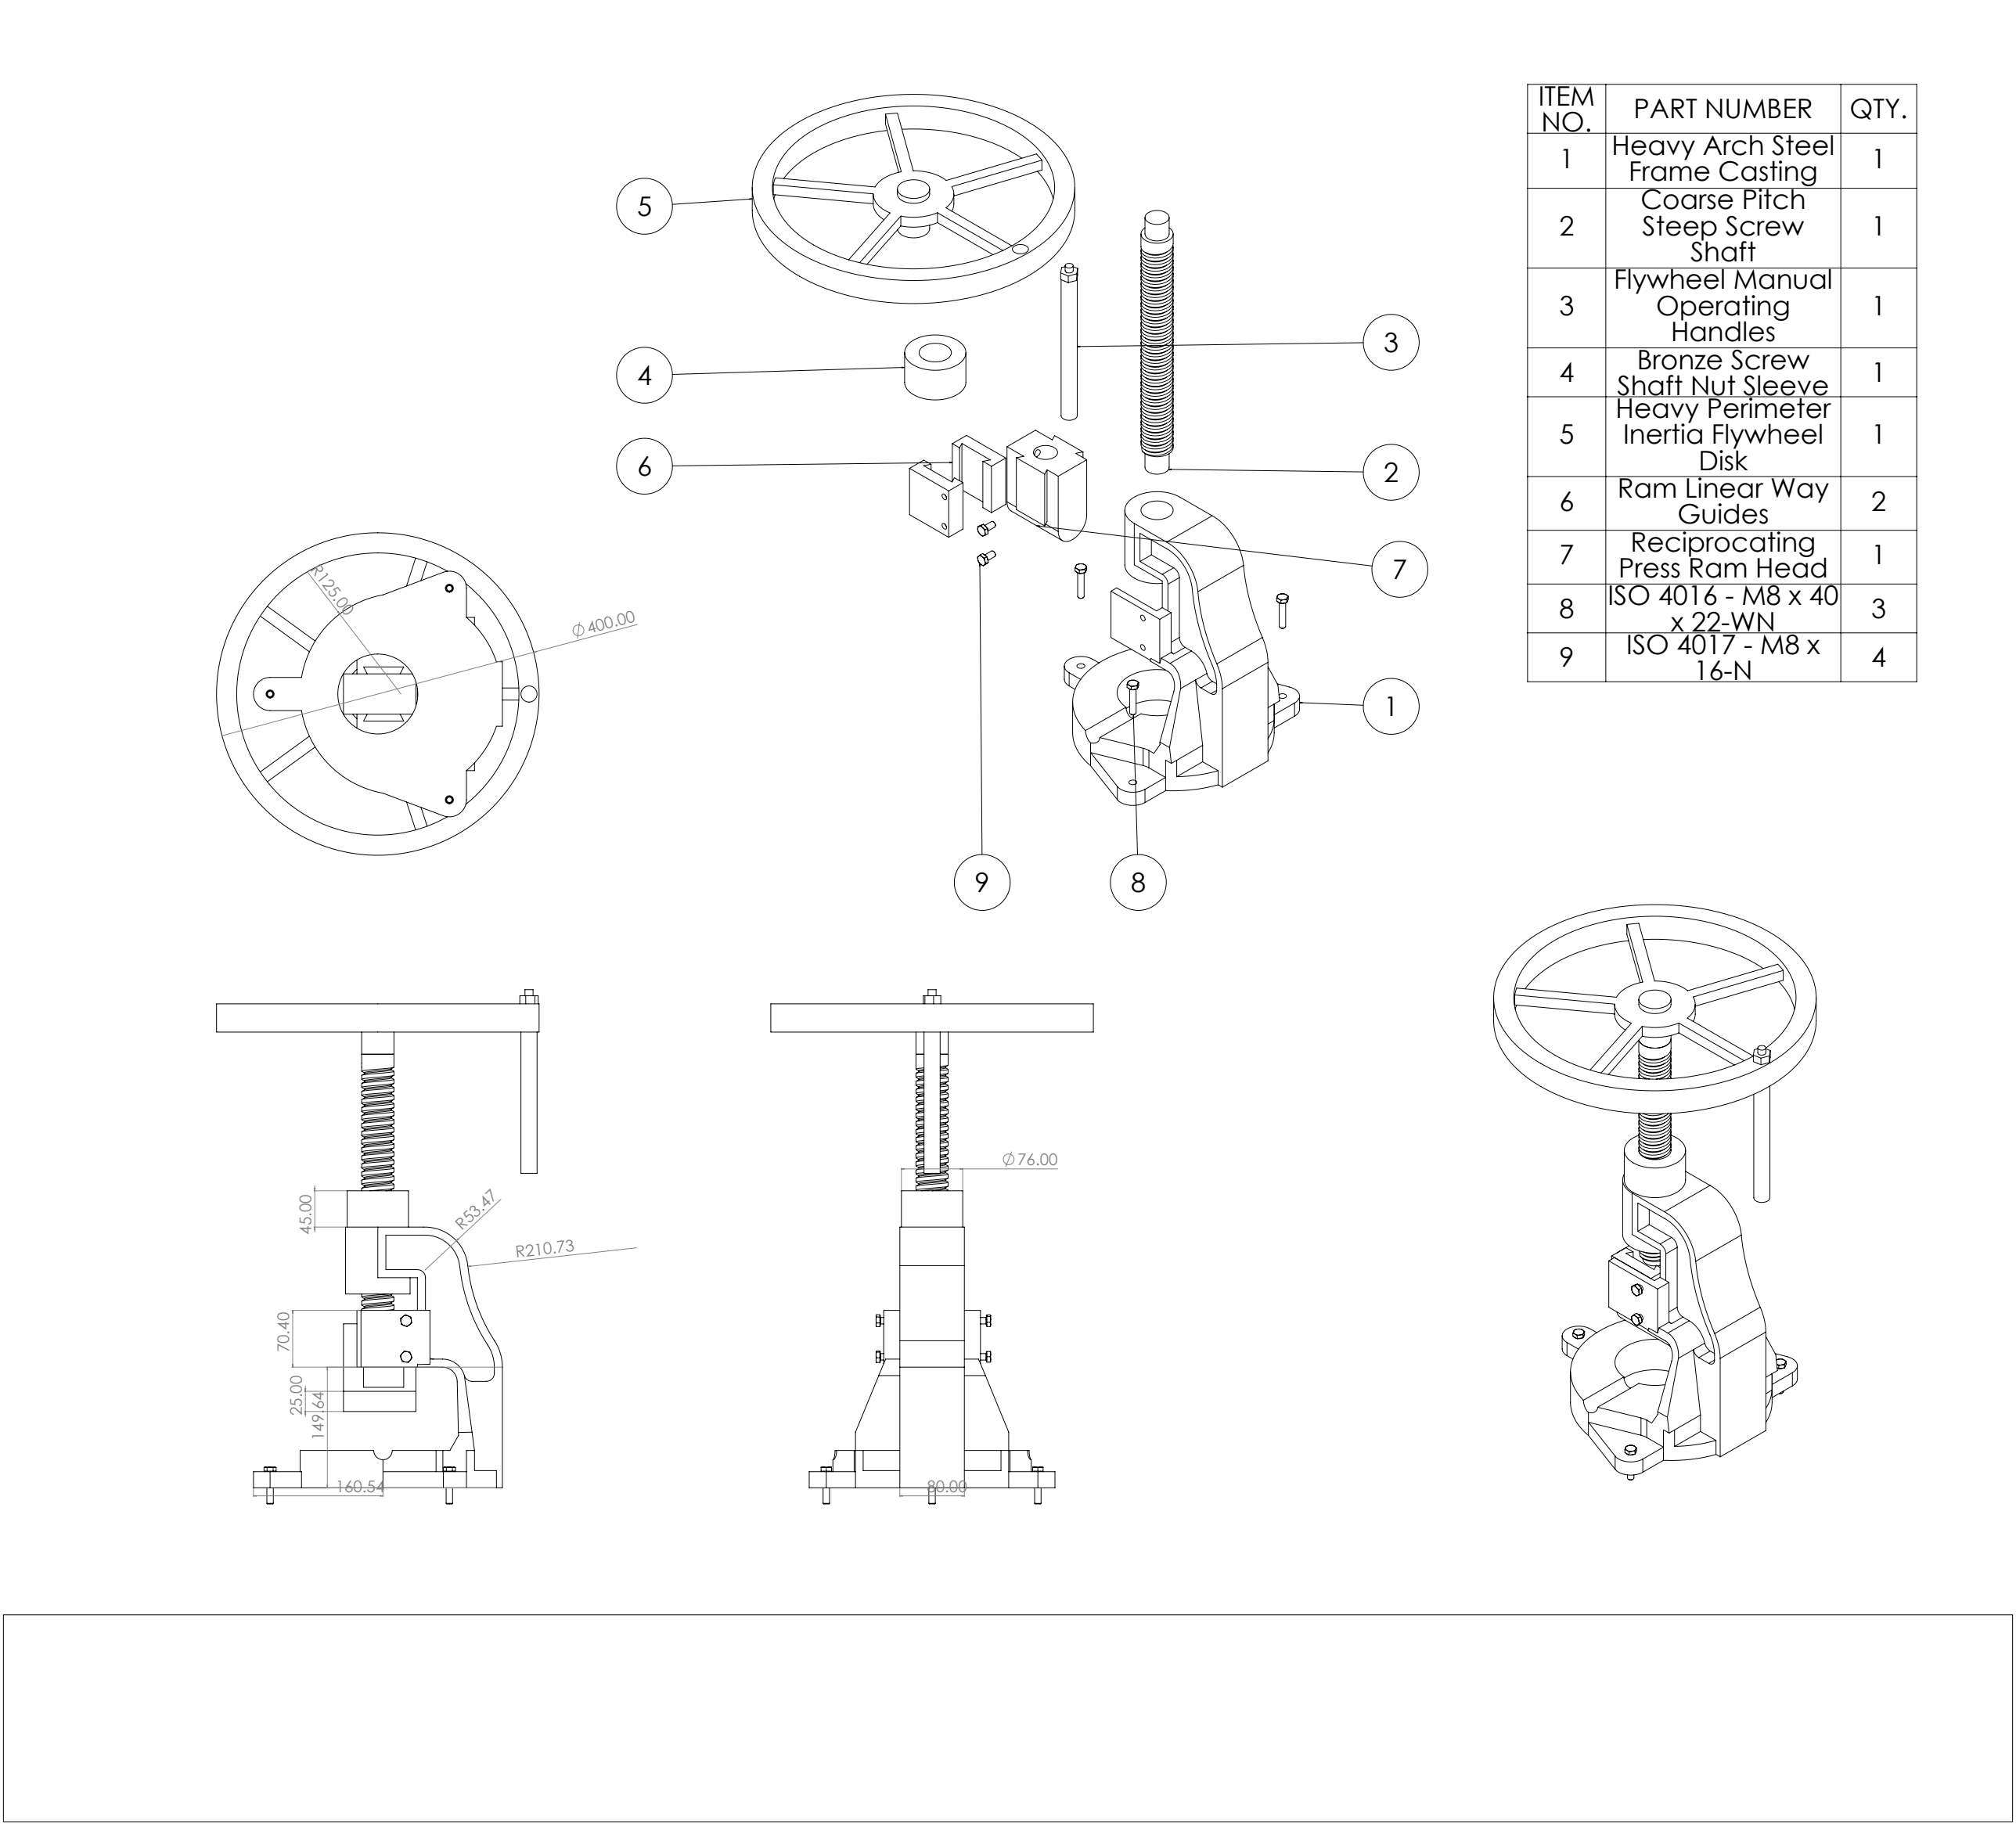
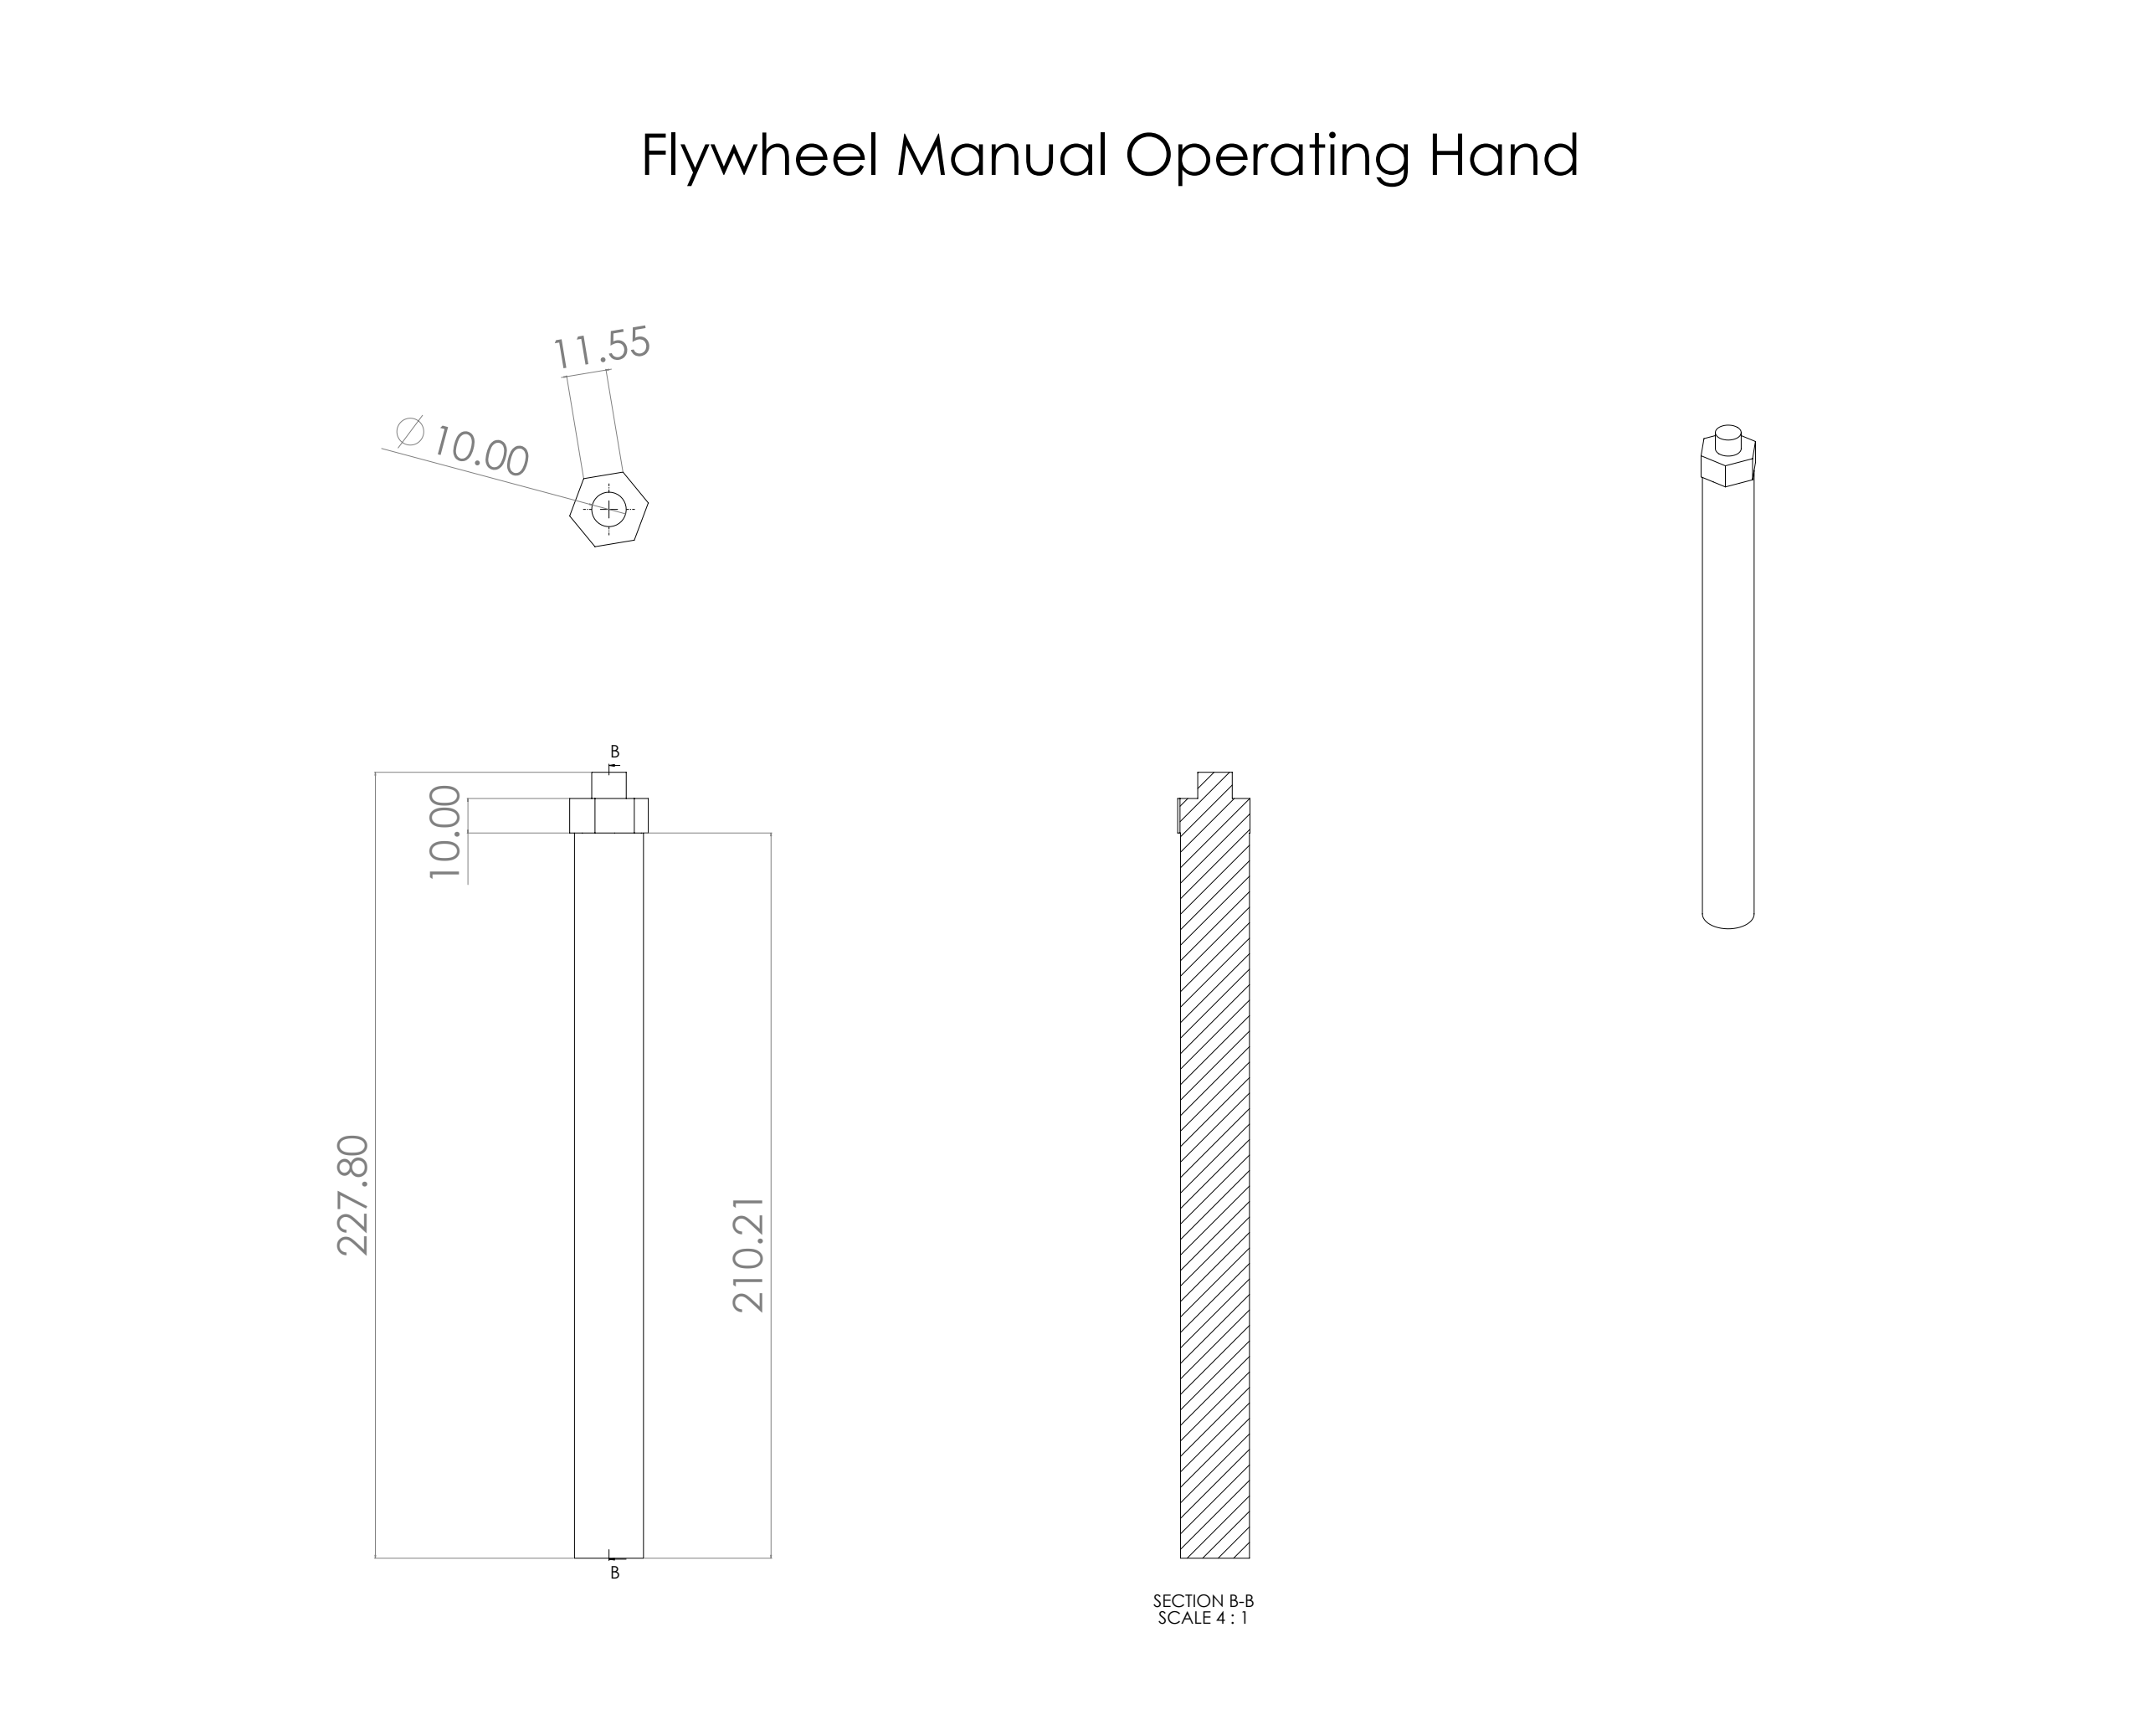
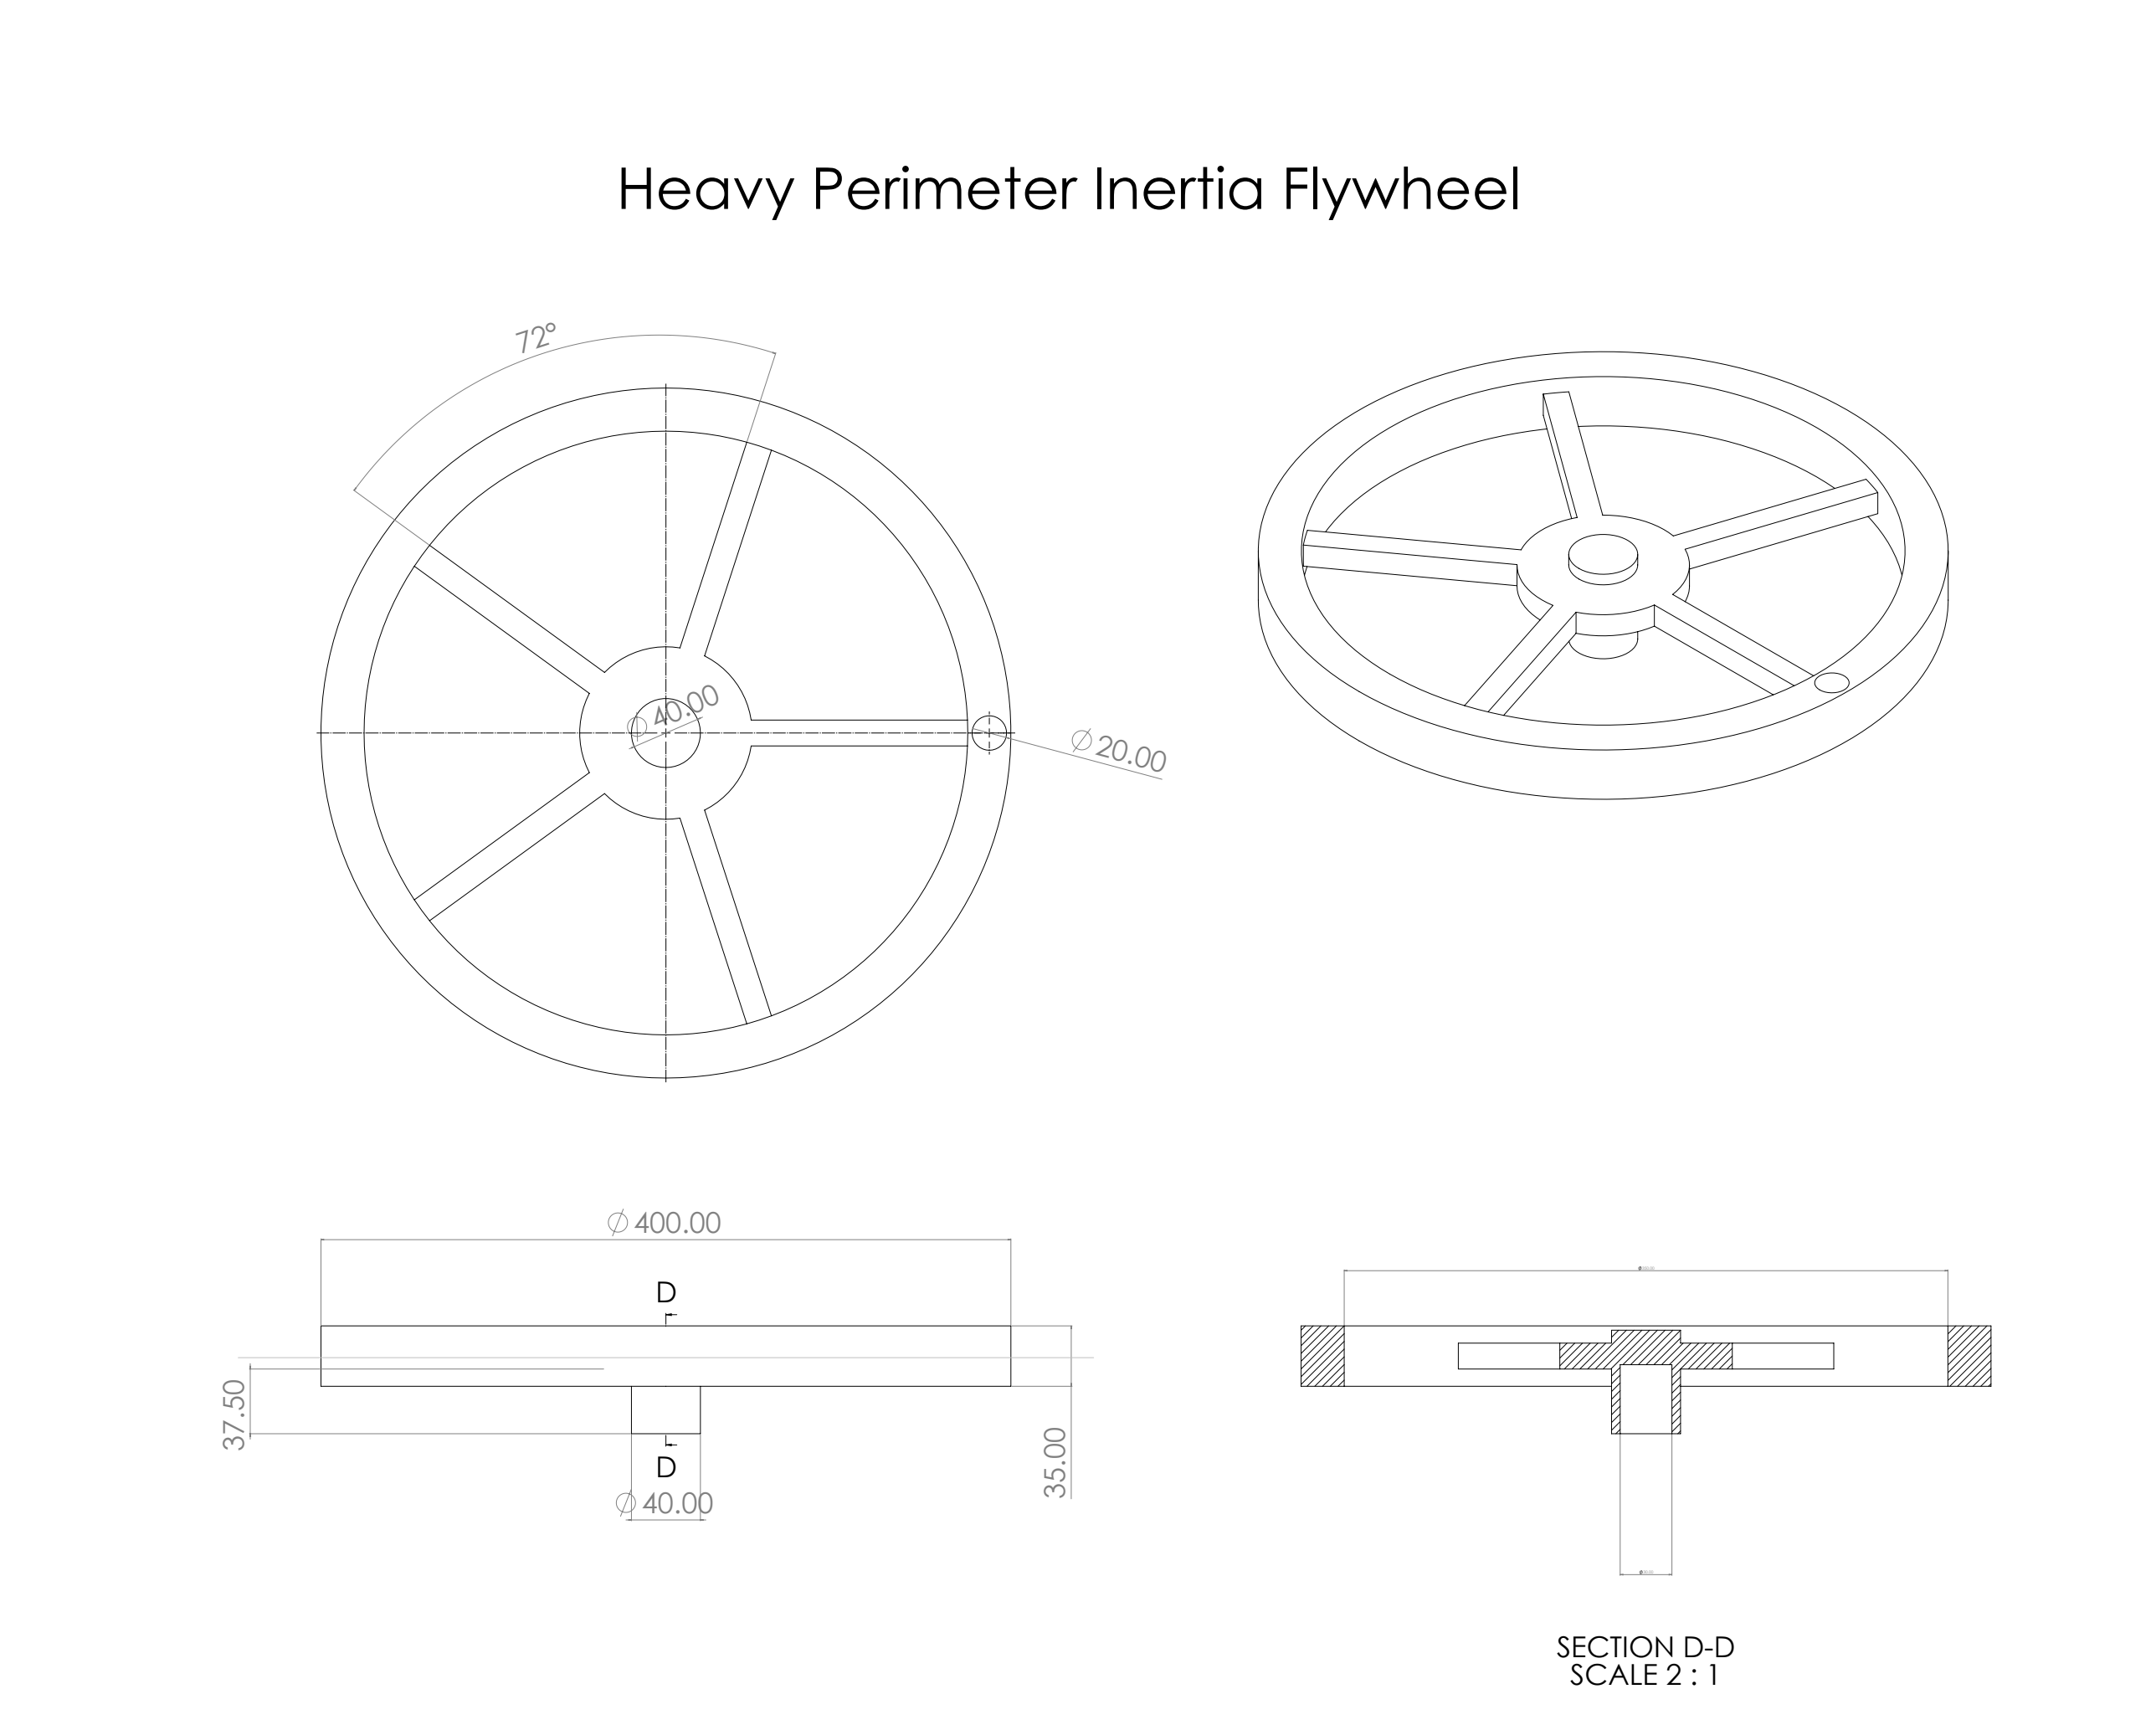
ISO-10303-21;
HEADER;
FILE_DESCRIPTION (('STEP AP214'),
    '1' );
FILE_NAME ('MAS-323',
    '2026-10-24T00:28:05',
    ( '' ),
    ( '' ),
    'SwSTEP 2.0',
    'SolidWorks 2025',
    '' );
FILE_SCHEMA (( 'AUTOMOTIVE_DESIGN' ));
ENDSEC;

DATA;
#1 = CARTESIAN_POINT ( 'NONE',  ( -40.53162694259543031, 272.6198905683720568, -11.84573899990672707 ) ) ;
#2 = CARTESIAN_POINT ( 'NONE',  ( -13.20868407381886200, 380.9948905683720568, -6.410867750099233042 ) ) ;
#3 = VECTOR ( 'NONE', #11444, 1000.000000000000000 ) ;
#4 = DIRECTION ( 'NONE',  ( 0.000000000000000000, -1.000000000000000000, 0.000000000000000000 ) ) ;
#5 = FACE_BOUND ( 'NONE', #9195, .T. ) ;
#6 = CARTESIAN_POINT ( 'NONE',  ( -10.20829729246297646, 267.6198905765655809, -7.653668647301794969 ) ) ;
#7 = CARTESIAN_POINT ( 'NONE',  ( -42.88789093042844058, 432.9323905683720000, -9.489475012073736337 ) ) ;
#8 = DIRECTION ( 'NONE',  ( -0.000000000000000000, -0.000000000000000000, -1.000000000000000000 ) ) ;
#9 = ORIENTED_EDGE ( 'NONE', *, *, #63, .F. ) ;
#10 = CARTESIAN_POINT ( 'NONE',  ( -47.16347859291445133, 436.6198905601784759, -7.653668647301793193 ) ) ;
#11 = ORIENTED_EDGE ( 'NONE', *, *, #16208, .F. ) ;
#12 = ORIENTED_EDGE ( 'NONE', *, *, #11019, .T. ) ;
#13 = VERTEX_POINT ( 'NONE', #14894 ) ;
#14 = CARTESIAN_POINT ( 'NONE',  ( -43.04716123355245827, 207.6569251493015429, -4.334626618252813479 ) ) ;
#15 = CARTESIAN_POINT ( 'NONE',  ( -40.01497788969912506, 298.8073905601784759, 16.95518130045146776 ) ) ;
#16 = FACE_OUTER_BOUND ( 'NONE', #20943, .T. ) ;
#17 = CARTESIAN_POINT ( 'NONE',  ( -40.53162694259543741, 334.1198905683720568, -11.84573899990672707 ) ) ;
#18 = CARTESIAN_POINT ( 'NONE',  ( -48.68588794268872277, 492.3073905765656946, 3.978247347593168115 ) ) ;
#19 = CARTESIAN_POINT ( 'NONE',  ( -25.35362745456398059, 366.6823905683720000, 16.75240474999998952 ) ) ;
#20 = CARTESIAN_POINT ( 'NONE',  ( -28.68588794268870856, 309.4948905765656377, -19.99999999999999289 ) ) ;
#21 = CARTESIAN_POINT ( 'NONE',  ( -11.93348319268872437, 388.5573905683719431, 3.332260488124728859 ) ) ;
#22 = CARTESIAN_POINT ( 'NONE',  ( -36.33955658999050087, 300.1198905765656377, -18.47759065022572855 ) ) ;
#23 = CARTESIAN_POINT ( 'NONE',  ( 20.42502041961814641, 160.1716627696692683, -50.00000000000000000 ) ) ;
#24 = CARTESIAN_POINT ( 'NONE',  ( -28.68588794268870146, 276.3698905683720000, 16.75240474999999307 ) ) ;
#25 = DIRECTION ( 'NONE',  ( 0.000000000000000000, 0.000000000000000000, 1.000000000000000000 ) ) ;
#26 = AXIS2_PLACEMENT_3D ( 'NONE', #1810, #8485, #15108 ) ;
#27 = CARTESIAN_POINT ( 'NONE',  ( -16.84014894278199392, 429.1198905683720000, 11.84573899990672530 ) ) ;
#28 = CARTESIAN_POINT ( 'NONE',  ( -33.09803238365465461, 52.74628974220605215, 120.5385558893279807 ) ) ;
#29 = CARTESIAN_POINT ( 'NONE',  ( -45.64106924314019409, 498.1823905601784759, 11.32908994701042538 ) ) ;
#30 = CARTESIAN_POINT ( 'NONE',  ( -10.76731745429009912, 56.85652257517428865, 118.3724535612433186 ) ) ;
#31 = CARTESIAN_POINT ( 'NONE',  ( -36.33955658999052218, 449.1198905601784759, 18.47759065022572500 ) ) ;
#32 =( GEOMETRIC_REPRESENTATION_CONTEXT ( 3 ) GLOBAL_UNCERTAINTY_ASSIGNED_CONTEXT ( ( #4204 ) ) GLOBAL_UNIT_ASSIGNED_CONTEXT ( ( #10723, #14002, #17024 ) ) REPRESENTATION_CONTEXT ( 'NONE', 'WORKASPACE' ) );
#33 = CARTESIAN_POINT ( 'NONE',  ( -35.09675569278794427, 343.4948905683720000, -15.47720386886985544 ) ) ;
#34 = CARTESIAN_POINT ( 'NONE',  ( -45.43829269268872650, 483.8698905683720568, 0.000000000000000000 ) ) ;
#35 = ORIENTED_EDGE ( 'NONE', *, *, #14468, .F. ) ;
#36 = CARTESIAN_POINT ( 'NONE',  ( -14.54375231895778597, 493.4948905601784759, -14.14213562373094746 ) ) ;
#37 = CARTESIAN_POINT ( 'NONE',  ( -11.93348319268871371, 298.8698905683720000, -2.051577885510841163E-15 ) ) ;
#38 = EDGE_CURVE ( 'NONE', #12347, #13852, #5030, .T. ) ;
#39 = ORIENTED_EDGE ( 'NONE', *, *, #13139, .T. ) ;
#40 = AXIS2_PLACEMENT_3D ( 'NONE', #19318, #13155, #16192 ) ;
#41 = VECTOR ( 'NONE', #20803, 1000.000000000000000 ) ;
#42 = FACE_OUTER_BOUND ( 'NONE', #15796, .T. ) ;
#43 = ORIENTED_EDGE ( 'NONE', *, *, #17610, .F. ) ;
#44 = CYLINDRICAL_SURFACE ( 'NONE', #20879, 19.99999999999999645 ) ;
#45 = VECTOR ( 'NONE', #2410, 999.9999999999998863 ) ;
#46 = CARTESIAN_POINT ( 'NONE',  ( -38.17536295476245556, 396.9323905683721136, 14.20200298773971781 ) ) ;
#47 = CARTESIAN_POINT ( 'NONE',  ( -42.82802356641967378, 478.4948905601784759, 14.14213562373094923 ) ) ;
#48 = PRODUCT_DEFINITION ( 'UNKNOWN', '', #8316, #8336 ) ;
#49 = SURFACE_SIDE_STYLE ('',( #161 ) ) ;
#50 = CARTESIAN_POINT ( 'NONE',  ( -35.09675569278795848, 415.7448905683720000, 15.47720386886985366 ) ) ;
#51 = CIRCLE ( 'NONE', #12122, 25.00000000000000711 ) ;
#52 = CARTESIAN_POINT ( 'NONE',  ( -44.16309181155858710, 453.2448905683720000, -6.410867750099231266 ) ) ;
#53 = APPLICATION_PROTOCOL_DEFINITION ( 'draft international standard', 'automotive_design', 1998, #17977 ) ;
#54 =( BOUNDED_CURVE ( )  B_SPLINE_CURVE ( 2, ( #11189, #17470, #6102, #14134, #19307, #19518, #7828, #9666, #17890, #9247, #17790, #20831, #12824, #19413, #5894, #9562, #16180 ),
 .UNSPECIFIED., .F., .T. ) 
 B_SPLINE_CURVE_WITH_KNOTS ( ( 3, 2, 2, 2, 2, 2, 2, 2, 3 ),
 ( 0.5937500000000002220, 0.5957031250000002220, 0.5976562500000002220, 0.5996093750000002220, 0.6015625000000002220, 0.6035156250000002220, 0.6054687500000002220, 0.6074218750000002220, 0.6093750000000002220 ),
 .UNSPECIFIED. ) 
 CURVE ( )  GEOMETRIC_REPRESENTATION_ITEM ( )  RATIONAL_B_SPLINE_CURVE ( ( 0.9999999999999977796, 0.9807852804032326510, 1.000000000000000000, 0.9807852804032304306, 1.000000000000000000, 0.9807852804032304306, 1.000000000000000000, 0.9807852804032304306, 1.000000000000000000, 0.9807852804032304306, 1.000000000000000000, 0.9807852804032304306, 1.000000000000000000, 0.9807852804032304306, 1.000000000000000000, 0.9807852804032282101, 1.000000000000002220 ) ) 
 REPRESENTATION_ITEM ( '' )  );
#55 = CARTESIAN_POINT ( 'NONE',  ( -28.68588794268875475, 600.7448905601785327, 0.000000000000000000 ) ) ;
#56 = DIRECTION ( 'NONE',  ( -1.191790137725560488E-16, 1.000000000000000000, -0.000000000000000000 ) ) ;
#57 = CARTESIAN_POINT ( 'NONE',  ( -40.01497788969913927, 393.5573905765656377, 16.95518130045146776 ) ) ;
#58 = CYLINDRICAL_SURFACE ( 'NONE', #7896, 15.00000000000000000 ) ;
#59 = CARTESIAN_POINT ( 'NONE',  ( 115.7989814974898337, 152.5259582928263740, 40.00000000000000000 ) ) ;
#60 = DIRECTION ( 'NONE',  ( 1.000000000000000000, 9.855701800883827197E-17, 0.000000000000000000 ) ) ;
#61 = CARTESIAN_POINT ( 'NONE',  ( -47.16347859291445843, 491.3698905765655809, -7.653668647301793193 ) ) ;
#62 = CARTESIAN_POINT ( 'NONE',  ( -11.93348319268873858, 500.3698905683720000, -2.051577885510841163E-15 ) ) ;
#63 = EDGE_CURVE ( 'NONE', #14197, #16401, #15913, .T. ) ;
#64 = AXIS2_PLACEMENT_3D ( 'NONE', #6317, #12505, #19097 ) ;
#65 = DIRECTION ( 'NONE',  ( -1.191790137725560488E-16, 1.000000000000000000, -0.000000000000000000 ) ) ;
#66 = VECTOR ( 'NONE', #19621, 1000.000000000000000 ) ;
#67 = CARTESIAN_POINT ( 'NONE',  ( -48.68588794268872277, 467.2448905601784759, 0.000000000000000000 ) ) ;
#68 = CARTESIAN_POINT ( 'NONE',  ( -22.30770786884145451, -343.0245277843623057, -122.9933582338429687 ) ) ;
#69 = CARTESIAN_POINT ( 'NONE',  ( -11.93348319268872615, 400.3698905683720000, -2.051577885510841163E-15 ) ) ;
#70 = CARTESIAN_POINT ( 'NONE',  ( 20.42502041961814641, 160.1716627696692683, 49.99999999999999289 ) ) ;
#71 = CARTESIAN_POINT ( 'NONE',  ( -22.27502019258946930, 222.2448905683720568, -15.47720386886985544 ) ) ;
#72 = CARTESIAN_POINT ( 'NONE',  ( -22.27502019258947641, 356.9948905683720000, 15.47720386886985189 ) ) ;
#73 = ADVANCED_FACE ( 'NONE', ( #292 ), #3940, .T. ) ;
#74 = VERTEX_POINT ( 'NONE', #5769 ) ;
#75 = CARTESIAN_POINT ( 'NONE',  ( -44.16309181155859420, 533.2448905683719431, -6.410867750099231266 ) ) ;
#76 = ORIENTED_EDGE ( 'NONE', *, *, #1697, .T. ) ;
#77 = CARTESIAN_POINT ( 'NONE',  ( -11.93348319268873148, 450.3698905683720000, -2.051577885510841163E-15 ) ) ;
#78 = CARTESIAN_POINT ( 'NONE',  ( -11.93348319268874036, 519.1823905683719431, -3.332260488124732856 ) ) ;
#79 = ORIENTED_EDGE ( 'NONE', *, *, #12757, .T. ) ;
#80 = COLOUR_RGB ( '',0.7921568627450980005, 0.8196078431372548767, 0.9333333333333333481 ) ;
#81 = CARTESIAN_POINT ( 'NONE',  ( -36.33955658999052218, 429.1198905601784759, 18.47759065022572500 ) ) ;
#82 = CARTESIAN_POINT ( 'NONE',  ( -45.43829269268872650, 493.8698905683720568, 0.000000000000000000 ) ) ;
#83 = ORIENTED_EDGE ( 'NONE', *, *, #15392, .F. ) ;
#84 = CARTESIAN_POINT ( 'NONE',  ( -13.20868407381887799, 499.4948905683720568, -6.410867750099233042 ) ) ;
#85 = CARTESIAN_POINT ( 'NONE',  ( -11.33174043645153262, 53.25345476394927857, -46.46619372074344767 ) ) ;
#86 = CARTESIAN_POINT ( 'NONE',  ( -40.01497788969914637, 440.4323905765656377, -16.95518130045146421 ) ) ;
#87 = CARTESIAN_POINT ( 'NONE',  ( 5.299999999999999822, 7.960204194457796463E-16, -6.500000000000000888 ) ) ;
#88 = CARTESIAN_POINT ( 'NONE',  ( -8.685887942688530927, 247.3073905765656093, -3.978247347592740013 ) ) ;
#89 = FACE_OUTER_BOUND ( 'NONE', #5371, .T. ) ;
#90 = DIRECTION ( 'NONE',  ( 0.000000000000000000, 0.000000000000000000, -1.000000000000000000 ) ) ;
#91 = DIRECTION ( 'NONE',  ( 1.854788578061058554E-16, 1.000000000000000000, 0.000000000000000000 ) ) ;
#92 = CARTESIAN_POINT ( 'NONE',  ( 3.458603197740078627, 135.1716627696692683, -33.59072564020503648 ) ) ;
#93 = CARTESIAN_POINT ( 'NONE',  ( -28.68588794268870856, 292.8698905683720568, -16.75240474999999307 ) ) ;
#94 = CARTESIAN_POINT ( 'NONE',  ( -10.76731745429010090, 56.85652257517428865, -152.3753892284480003 ) ) ;
#95 = CARTESIAN_POINT ( 'NONE',  ( -14.54375231895775400, 260.9948905601784759, 14.14213562373094568 ) ) ;
#96 = DIRECTION ( 'NONE',  ( -1.000000000000000000, 0.000000000000000000, 0.000000000000000000 ) ) ;
#97 = PRESENTATION_LAYER_ASSIGNMENT (  '', '', ( #13555 ) ) ;
#98 = CARTESIAN_POINT ( 'NONE',  ( -16.84014894278200458, 509.1198905683720568, 11.84573899990672530 ) ) ;
#99 = CARTESIAN_POINT ( 'NONE',  ( -32.66413529028187668, 369.4323905601784190, 19.99999999999999289 ) ) ;
#100 = CARTESIAN_POINT ( 'NONE',  ( -28.68588794268872277, 230.8848358243226073, -40.00000000000000000 ) ) ;
#101 = ORIENTED_EDGE ( 'NONE', *, *, #3009, .T. ) ;
#102 = CARTESIAN_POINT ( 'NONE',  ( -14.48388495494900852, 469.4323905683720568, 9.489475012073732785 ) ) ;
#103 = CARTESIAN_POINT ( 'NONE',  ( -42.88789093042842637, 274.8073905683720000, 9.489475012073736337 ) ) ;
#104 = VECTOR ( 'NONE', #10753, 1000.000000000000000 ) ;
#105 = ORIENTED_EDGE ( 'NONE', *, *, #199, .F. ) ;
#106 = CARTESIAN_POINT ( 'NONE',  ( 0.000000000000000000, -5.629165124598843661, 3.250000000000012434 ) ) ;
#107 = EDGE_CURVE ( 'NONE', #16081, #2296, #14541, .T. ) ;
#108 = CARTESIAN_POINT ( 'NONE',  ( -10.20829729246297291, 237.6198905765656377, -7.653668647301794969 ) ) ;
#109 = CARTESIAN_POINT ( 'NONE',  ( -28.68588794268870501, 309.7448905601785327, 19.99999999999999289 ) ) ;
#110 = CARTESIAN_POINT ( 'NONE',  ( -48.68588794268872988, 537.2448905601785327, 0.000000000000000000 ) ) ;
#111 = CARTESIAN_POINT ( 'NONE',  ( 18.20947592957839589, 585.7448905601785327, 168.5995991907681457 ) ) ;
#112 = CARTESIAN_POINT ( 'NONE',  ( -44.16309181155856578, 273.2448905683720568, -6.410867750099231266 ) ) ;
#113 = EDGE_CURVE ( 'NONE', #8154, #14441, #20281, .T. ) ;
#114 = CARTESIAN_POINT ( 'NONE',  ( -11.93348319268872260, 350.6823905683720000, -3.332260488124732856 ) ) ;
#115 = EDGE_CURVE ( 'NONE', #339, #18802, #16604, .T. ) ;
#116 = CARTESIAN_POINT ( 'NONE',  ( 69.79185940953689737, 142.2976266388001250, 69.11456258820065557 ) ) ;
#117 = AXIS2_PLACEMENT_3D ( 'NONE', #15282, #17003, #20238 ) ;
#118 = CARTESIAN_POINT ( 'NONE',  ( -19.19641293061498999, 427.3073905683720568, 14.20200298773971426 ) ) ;
#119 = CARTESIAN_POINT ( 'NONE',  ( -14.54375231895778420, 510.9948905601784190, 14.14213562373094568 ) ) ;
#120 = EDGE_LOOP ( 'NONE', ( #6723, #18593, #5949, #4393 ) ) ;
#121 = CARTESIAN_POINT ( 'NONE',  ( -14.54375231895777354, 420.9948905601784759, 14.14213562373094568 ) ) ;
#122 = ADVANCED_FACE ( 'NONE', ( #15530 ), #711, .F. ) ;
#123 = ORIENTED_EDGE ( 'NONE', *, *, #2940, .T. ) ;
#124 = CARTESIAN_POINT ( 'NONE',  ( 0.2573354458087829810, 6.889406814520511624, -1.067197363239223762 ) ) ;
#125 = ORIENTED_EDGE ( 'NONE', *, *, #1712, .T. ) ;
#126 = VERTEX_POINT ( 'NONE', #20705 ) ;
#127 = CARTESIAN_POINT ( 'NONE',  ( -45.43829269268873361, 525.3698905683720568, 0.000000000000000000 ) ) ;
#128 = CARTESIAN_POINT ( 'NONE',  ( -36.33955658999050087, 305.3698905601784759, -18.47759065022572855 ) ) ;
#129 = FACE_OUTER_BOUND ( 'NONE', #19320, .T. ) ;
#130 = CIRCLE ( 'NONE', #6669, 6.500000000000000888 ) ;
#131 = CARTESIAN_POINT ( 'NONE',  ( -35.09675569278794427, 343.4948905683720000, -15.47720386886985544 ) ) ;
#132 = ORIENTED_EDGE ( 'NONE', *, *, #11871, .F. ) ;
#133 = CARTESIAN_POINT ( 'NONE',  ( -45.64106924314020119, 481.0573905765656377, -11.32908994701042715 ) ) ;
#134 = CARTESIAN_POINT ( 'NONE',  ( -38.17536295476245556, 362.3073905683719431, -14.20200298773971426 ) ) ;
#135 = VECTOR ( 'NONE', #18235, 1000.000000000000000 ) ;
#136 = CARTESIAN_POINT ( 'NONE',  ( -14.48388495494899963, 377.9323905683720000, 9.489475012073731008 ) ) ;
#137 = CARTESIAN_POINT ( 'NONE',  ( -14.54375231895775933, 305.7448905765656377, 14.14213562373094568 ) ) ;
#138 = DIRECTION ( 'NONE',  ( 1.191790137725560488E-16, -1.000000000000000000, -0.000000000000000000 ) ) ;
#139 = CARTESIAN_POINT ( 'NONE',  ( -32.01814843081343298, 271.6823905683720000, -16.75240474999999307 ) ) ;
#140 = CARTESIAN_POINT ( 'NONE',  ( -24.70764059509555821, 440.0573905601785327, 19.99999999999998934 ) ) ;
#141 = CARTESIAN_POINT ( 'NONE',  ( -28.68588794268871922, 427.8698905683720568, 16.75240474999999307 ) ) ;
#142 = DIRECTION ( 'NONE',  ( 1.191790137725560488E-16, -1.000000000000000000, -0.000000000000000000 ) ) ;
#143 = CARTESIAN_POINT ( 'NONE',  ( -48.68588794268881514, 497.5573905601784190, 3.978247347592954952 ) ) ;
#144 = CARTESIAN_POINT ( 'NONE',  ( -14.31911992702480241, 600.7448905601785327, 19.70857778461545351 ) ) ;
#145 = PRODUCT_DEFINITION_CONTEXT ( 'detailed design', #14845, 'design' ) ;
#146 = CARTESIAN_POINT ( 'NONE',  ( 20.42502041961814641, 160.1716627696692683, 61.32762281133329196 ) ) ;
#147 = VECTOR ( 'NONE', #5877, 1000.000000000000000 ) ;
#148 = CARTESIAN_POINT ( 'NONE',  ( -13.20868407381885845, 340.9948905683720000, -6.410867750099233042 ) ) ;
#149 = CARTESIAN_POINT ( 'NONE',  ( -32.01814843081346140, 486.0573905683721136, 16.75240474999999307 ) ) ;
#150 = VECTOR ( 'NONE', #6440, 1000.000000000000000 ) ;
#151 = ORIENTED_EDGE ( 'NONE', *, *, #2836, .T. ) ;
#152 = CARTESIAN_POINT ( 'NONE',  ( -28.68588794268872633, 489.7448905601784759, 19.99999999999999289 ) ) ;
#153 = CARTESIAN_POINT ( 'NONE',  ( -40.53162694259543031, 312.6198905683720000, -11.84573899990672707 ) ) ;
#154 = VECTOR ( 'NONE', #10153, 1000.000000000000000 ) ;
#155 = ORIENTED_EDGE ( 'NONE', *, *, #15237, .F. ) ;
#156 = CARTESIAN_POINT ( 'NONE',  ( -54.57497958038185004, 160.1716627696692683, 49.99999999999999289 ) ) ;
#157 = EDGE_LOOP ( 'NONE', ( #5136, #14998, #4320, #2465 ) ) ;
#158 = CARTESIAN_POINT ( 'NONE',  ( 4.700000000000000178, 6.500000000000000888, 0.000000000000000000 ) ) ;
#159 = CARTESIAN_POINT ( 'NONE',  ( -42.88789093042844058, 394.4323905683720000, -9.489475012073734561 ) ) ;
#160 = CARTESIAN_POINT ( 'NONE',  ( -14.54375231895777709, 445.7448905765656377, 14.14213562373094568 ) ) ;
#161 = SURFACE_STYLE_FILL_AREA ( #18197 ) ;
#162 = CARTESIAN_POINT ( 'NONE',  ( -22.27502019258948351, 416.9948905683720000, 15.47720386886985189 ) ) ;
#163 = CARTESIAN_POINT ( 'NONE',  ( -38.17536295476243424, 256.9323905683720568, 14.20200298773971781 ) ) ;
#164 = CARTESIAN_POINT ( 'NONE',  ( -38.17536295476246266, 442.3073905683721136, -14.20200298773971426 ) ) ;
#165 = APPLICATION_PROTOCOL_DEFINITION ( 'draft international standard', 'automotive_design', 1998, #13733 ) ;
#166 = CARTESIAN_POINT ( 'NONE',  ( -48.68588794268873698, 573.2448905601785327, 0.000000000000000000 ) ) ;
#167 = CARTESIAN_POINT ( 'NONE',  ( -10.20829729246298534, 356.3698905765655809, 7.653668647301790529 ) ) ;
#168 = DIRECTION ( 'NONE',  ( 0.000000000000000000, 0.000000000000000000, -1.000000000000000000 ) ) ;
#169 = CARTESIAN_POINT ( 'NONE',  ( -14.54375231895777354, 388.2448905765655809, -14.14213562373094746 ) ) ;
#170 = CARTESIAN_POINT ( 'NONE',  ( -32.66413529028187668, 429.8073905765656946, -19.99999999999999289 ) ) ;
#171 = DIRECTION ( 'NONE',  ( 1.000000000000000000, 0.000000000000000000, 0.000000000000000000 ) ) ;
#172 = CARTESIAN_POINT ( 'NONE',  ( -22.27502019258949417, 498.4948905683720568, 15.47720386886985189 ) ) ;
#173 = EDGE_CURVE ( 'NONE', #3963, #2116, #12492, .T. ) ;
#174 = LINE ( 'NONE', #10093, #7830 ) ;
#175 = CARTESIAN_POINT ( 'NONE',  ( -40.01497788969915348, 465.6823905601785896, -16.95518130045146421 ) ) ;
#176 = CARTESIAN_POINT ( 'NONE',  ( -14.54375231895777354, 420.9948905601784759, 14.14213562373094568 ) ) ;
#177 = CARTESIAN_POINT ( 'NONE',  ( -11.93348319268872615, 400.6823905683720568, -3.332260488124732856 ) ) ;
#178 = CARTESIAN_POINT ( 'NONE',  ( -47.16347859291445843, 471.3698905765656377, -7.653668647301793193 ) ) ;
#179 = EDGE_CURVE ( 'NONE', #20702, #11681, #8806, .T. ) ;
#180 = CARTESIAN_POINT ( 'NONE',  ( -42.88789093042841927, 236.3073905683720284, 9.489475012073736337 ) ) ;
#181 = CARTESIAN_POINT ( 'NONE',  ( -35.09675569278795138, 365.7448905683720568, 15.47720386886985366 ) ) ;
#182 = VERTEX_POINT ( 'NONE', #608 ) ;
#183 = CARTESIAN_POINT ( 'NONE',  ( -16.84014894278200813, 527.6198905683719431, 11.84573899990672530 ) ) ;
#184 = ORIENTED_EDGE ( 'NONE', *, *, #5125, .F. ) ;
#185 = CARTESIAN_POINT ( 'NONE',  ( -35.09675569278795848, 447.2448905683720000, 15.47720386886985366 ) ) ;
#186 =( BOUNDED_CURVE ( )  B_SPLINE_CURVE ( 2, ( #15683, #18905, #9166, #8954, #869, #19445, #2803, #4526, #19338, #8177, #16322, #1390, #12644, #11113, #16106, #17715, #7966, #3227, #12748, #9388, #20969, #19235, #11001, #14702, #1604, #16006, #4629, #6032, #9702, #21278, #1189, #19652, #11223, #18032, #12856, #14808, #9803, #4832, #1496, #17820, #3012, #6451, #7759, #4419, #17612, #2913, #9493, #16426, #14385, #6138, #1283, #7861, #14489, #21070, #6244, #9596, #16213, #8072, #12959, #19548, #14595, #13067, #11432, #21177, #6349, #4729, #11326, #17920, #3118, #15134, #11654, #3650, #13178, #3748, #8400, #11760, #18356, #8721, #18246, #1830, #8286, #19984, #15026, #16753, #98, #20097, #13397, #18136, #19875, #13290, #2139, #10231, #1940, #6557, #5050, #10021, #3438, #8506, #18566, #6670, #3330, #16531, #19763, #4947, #8608, #16958, #9912, #5164, #20768, #16855, #15231, #1717, #13612, #3545, #11969, #6776, #11547, #10336, #20198, #2039, #10132, #14915, #16646, #425, #315, #209, #6883, #13503, #5266, #5365, #11868, #18461, #6991, #10875, #2352, #10445, #631, #10552, #740, #12189, #5585, #7091, #5797, #13712, #20306, #17173, #18775, #8932, #17275, #12296, #15557, #5689, #9041, #529, #12403, #4292, #955, #17481, #2563, #15766, #15347, #3962, #7306, #7521, #19110, #13933, #20522, #9145, #18884, #2669, #4071, #10655, #14146, #2460, #8827, #20732, #18666, #5476, #12074, #15662, #7197, #848, #13819, #7413, #3856, #5906, #12515, #17067, #2250, #15445, #14039, #18994, #20621, #20410, #4178, #10767, #17382, #21258, #1063, #15874, #16082, #16189, #2989, #18007, #17898, #19213, #1163, #4500, #6326, #4606, #4810, #20842, #11404, #1261, #21154, #7838, #11089, #11198, #9366, #7938, #14466, #4705, #21048, #6114, #17799, #6216, #1367, #7629, #15981, #19314, #3093, #9572, #4396, #13040, #12832, #10978, #14256, #6014, #9675, #9257, #12623, #2886, #17694, #20944, #11301, #17588, #2780, #19421, #7735, #16299, #1472, #14365, #8048, #9470, #12725, #14569, #12940, #19526, #14680, #6424, #19630, #3201, #8878, #8376, #18328, #19739, #20465, #11629, #4923, #9887, #19851, #9993, #77, #14890, #6644, #5242, #13477, #10105, #6534, #10497, #14999, #5139, #185, #5028, #6753, #3518, #9779, #290, #13876, #21366, #18113, #2297, #11520, #13371, #16727, #20070, #15496, #18223, #13265, #3416, #11842, #17118, #1807, #682, #16617, #12244, #7248, #5635, #6859, #19961, #16404, #11738, #1915, #8483, #15106, #18438, #1581, #3625, #3309, #8152, #14780, #16511, #13151, #1690, #8261, #12491, #1034, #12597, #2644, #17455, #9230, #7813, #16062, #12700, #9120, #12805, #10954, #14542, #17564, #6193, #17774, #20919, #12078, #2861, #16165, #19397, #1341, #14443, #4581, #5478, #19189, #20704, #15850, #21024, #4368, #1139, #14229, #9332, #14339, #6086, #19081, #7914, #18967, #15742, #4149, #4264, #7598, #5878, #20817, #5987, #929, #1239, #19291, #4477, #10741, #10851, #11172, #11060, #17355, #2967, #2755, #17668, #9546, #9445, #15953, #2537, #7495, #14118, #7712, #11494, #18091, #8456, #17979, #1556, #8023, #19933, #13346, #3178, #3493, #3067, #1449, #17875, #19608, #13015, #1889, #9972, #16487, #6302, #4784, #9758, #11381, #1669, #18303, #6402, #12913, #16381, #8126, #14759, #8238, #10079, #21343, #19714, #16273, #19503, #4682, #8348, #16700, #9651, #4897, #21128, #3393, #14972, #14655, #5111, #3286, #11711, #6511, #11275, #21236, #13127, #16591, #9860, #14868, #46, #1781, #6618, #13239, #19829, #5004, #11605, #18195, #159, #6730, #10183, #10609, #2089, #16804, #370, #10288, #482, #11919, #13880, #6833, #5532, #13449, #20040, #16909, #5319, #8670, #17014, #12025, #15294, #5425, #8781, #267, #12138, #4015, #687, #17227, #2301, #15501, #2409, #18513, #3700, #7253, #7045, #8563, #8885, #18410, #15081, #5217, #13665, #6939, #11816, #3599, #1995, #15185, #13563, #20252, #20151, #18618, #20471, #2196, #18724, #3804, #5640, #10395, #3912, #10502, #12248, #15397, #578, #7147, #13770, #18831, #20358, #17123, #12673, #798, #12779, #17435, #4345, #4558, #20573, #11145, #1010, #20895, #7576, #10825, #10928, #9098, #7686, #14202, #5740, #7466, #902, #17750, #19268, #17538, #15924, #7364, #15611, #15826, #2729, #6169, #9309, #20678, #4448, #13991, #19372, #2619, #20792, #5958, #8989, #5853, #9199, #17330, #7787, #1217, #12458, #12352, #10710, #18939, #11034, #12573, #19057, #1115, #19167, #14315, #4124, #15718, #4240, #2837, #6063, #2513, #14097, #17643, #9419, #16039, #14419, #21001, #19798, #8322, #17953, #12988, #14629, #4978, #2941, #16137, #8101, #6276, #11577, #18168, #1320, #16565, #19580, #11251, #17848, #7891, #13214, #19686, #1640, #19904, #6591, #3044, #3365, #13100, #3259, #9520, #7997, #9945, #1750, #4760, #14945, #131, #14519, #6704, #21102, #14841, #12890, #19480, #13321, #14731, #11686, #21312, #5085, #4660, #9627, #16246, #1423, #11356, #21214, #6379, #16354, #3151, #9732, #1531, #6484, #4871, #11466, #18064, #9835, #16458, #8213, #17, #5397, #10163, #20334, #15269, #3574, #20126, #20441, #10476, #17097, #3887, #10053, #12106, #20227, #15375, #348, #8856, #18385, #5506, #10261, #18700, #13537, #7227, #8538, #6912, #2277, #3678, #11789, #15477, #239, #13850, #5615, #15161, #16781, #18277, #3465, #6808, #16677, #663, #1863, #8435, #15057, #13425, #12001, #553, #5293, #20017, #5193, #7122, #13748, #1967, #11896, #18489, #16882, #18592, #2066, #3778, #8641, #452, #7018, #13641, #10366, #16991, #2171, #8755, #14394, #4216, #2706, #10798, #14069, #7552, #12325, #10904, #17414, #8964, #10686, #4098, #14177, #9176, #4321, #10579, #18913, #879, #6042, #20767, #770, #16015, #2596, #7335, #18806, #17202, #20877, #7768, #15587, #15801, #12223, #15903, #7662, #3988, #2381, #988, #13968, #14290, #12651, #20551, #4428, #7443, #5717, #17305, #2488, #1094, #5935, #9071, #5824, #15692, #20654, #17621, #12550, #19144, #12434, #19030, #19245, #11012, #17515, #2812, #9396, #9287, #1197, #20978, #18040, #19347, #4535, #7976, #17828, #1400, #8081, #3126, #18145, #9501, #16115, #11121, #16223, #9922, #3022, #1292, #4738, #6146, #9812, #5558, #2921, #19772, #11335, #3340, #12967, #14925, #16541, #4957, #14603, #14498, #21081, #17726, #16435, #1506, #12758, #21186, #6253, #7869, #11557, #17929, #21287, #12864, #1726, #6357, #19454, #4637, #19557, #9711, #11231, #8298, #9604, #3236, #16331, #14711, #6460, #13076, #19662, #4841, #11440, #1614, #8187, #14817, #6568, #13188, #8833, #5484, #13298, #8729, #1947, #19884, #11768, #20104, #18675, #3657, #15034, #3863, #1841, #11664, #19993, #18363, #8619, #15243, #20207, #11977, #10345, #2148, #4740, #16225, #12969, #3024, #11558, #1616, #8188, #18255, #1402, #3342, #14818, #6255, #9923, #14606, #19456, #4864, #9813, #3446, #16542, #4639, #21188, #11337, #6462, #13078, #16117, #9713, #16333, #9606, #6679, #13299, #19665, #19885, #6359, #11442, #18043, #1727, #3237, #16436, #6569, #13189, #19773, #5061, #11665, #15143, #11981, #7207, #16760, #6787, #3554, #8837, #5172, #432, #2151, #6999, #538, #8732, #5596, #13725, #10143, #5487, #20209, #10348, #12200, #18470, #11769, #1948, #5274, #16865, #6892, #325, #13512, #12086, #20315, #16971, #13405, #17076, #15245, #18787, #13621, #10456, #641, #19994, #16656, #7104, #20421, #2259, #10030, #18678, #15457, #1842, #2048, #8516, #20105, #3866, #8622, #5375, #3658, #18575, #3758, #15357, #11878, #13829, #8410, #18364, #15035, #10241, #218, #4081, #859, #7423, #20532, #20855, #10886, #17493, #6129, #10667, #12635, #2684, #2363, #6025, #17286, #10561, #1177, #19121, #15673, #7645, #17184, #7748, #12414, #15780, #968, #12737, #14050, #5807, #12305, #2793, #17601, #20633, #14377, #7316 ),
 .UNSPECIFIED., .F., .T. ) 
 B_SPLINE_CURVE_WITH_KNOTS ( ( 3, 2, 2, 2, 2, 2, 2, 2, 2, 2, 2, 2, 2, 2, 2, 2, 2, 2, 2, 2, 2, 2, 2, 2, 2, 2, 2, 2, 2, 2, 2, 2, 2, 2, 2, 2, 2, 2, 2, 2, 2, 2, 2, 2, 2, 2, 2, 2, 2, 2, 2, 2, 2, 2, 2, 2, 2, 2, 2, 2, 2, 2, 2, 2, 2, 2, 2, 2, 2, 2, 2, 2, 2, 2, 2, 2, 2, 2, 2, 2, 2, 2, 2, 2, 2, 2, 2, 2, 2, 2, 2, 2, 2, 2, 2, 2, 2, 2, 2, 2, 2, 2, 2, 2, 2, 2, 2, 2, 2, 2, 2, 2, 2, 2, 2, 2, 2, 2, 2, 2, 2, 2, 2, 2, 2, 2, 2, 2, 2, 2, 2, 2, 2, 2, 2, 2, 2, 2, 2, 2, 2, 2, 2, 2, 2, 2, 2, 2, 2, 2, 2, 2, 2, 2, 2, 2, 2, 2, 2, 2, 2, 2, 2, 2, 2, 2, 2, 2, 2, 2, 2, 2, 2, 2, 2, 2, 2, 2, 2, 2, 2, 2, 2, 2, 2, 2, 2, 2, 2, 2, 2, 2, 2, 2, 2, 2, 2, 2, 2, 2, 2, 2, 2, 2, 2, 2, 2, 2, 2, 2, 2, 2, 2, 2, 2, 2, 2, 2, 2, 2, 2, 2, 2, 2, 2, 2, 2, 2, 2, 2, 2, 2, 2, 2, 2, 2, 2, 2, 2, 2, 2, 2, 2, 2, 2, 2, 2, 2, 2, 2, 2, 2, 2, 2, 2, 2, 2, 2, 2, 2, 2, 2, 2, 2, 2, 2, 2, 2, 2, 2, 2, 2, 2, 2, 2, 2, 2, 2, 2, 2, 2, 2, 2, 2, 2, 2, 2, 2, 2, 2, 2, 2, 2, 2, 2, 2, 2, 2, 2, 2, 2, 2, 2, 2, 2, 2, 2, 2, 2, 2, 2, 2, 2, 2, 2, 2, 2, 2, 2, 2, 2, 2, 2, 2, 2, 2, 2, 2, 2, 2, 2, 2, 2, 2, 2, 2, 2, 2, 2, 2, 2, 2, 2, 2, 2, 2, 2, 2, 2, 2, 2, 2, 2, 2, 2, 2, 2, 2, 2, 2, 2, 2, 2, 2, 2, 2, 2, 2, 2, 2, 2, 2, 2, 2, 2, 2, 2, 2, 2, 2, 2, 2, 2, 2, 2, 2, 2, 2, 2, 2, 2, 2, 2, 2, 2, 2, 2, 2, 2, 2, 2, 2, 2, 2, 2, 2, 2, 2, 2, 2, 2, 2, 2, 2, 2, 2, 2, 2, 2, 2, 2, 2, 2, 2, 2, 2, 2, 2, 2, 2, 2, 2, 2, 2, 2, 2, 2, 2, 2, 2, 2, 2, 2, 2, 2, 2, 2, 2, 2, 2, 2, 2, 2, 2, 2, 2, 2, 2, 2, 2, 2, 2, 2, 2, 2, 2, 2, 2, 2, 2, 2, 2, 2, 2, 2, 2, 2, 2, 2, 2, 2, 2, 2, 2, 2, 2, 2, 2, 2, 2, 2, 2, 2, 2, 2, 2, 2, 2, 2, 3 ),
 ( 0.000000000000000000, 0.001953125000000000000, 0.003906250000000000000, 0.005859374999999999133, 0.007812500000000000000, 0.009765625000000000000, 0.01171874999999999827, 0.01367187500000000000, 0.01562500000000000000, 0.01757812500000000000, 0.01953125000000000000, 0.02148437500000000000, 0.02343749999999999653, 0.02539062500000000000, 0.02734375000000000000, 0.02929687500000000000, 0.03125000000000000000, 0.03320312500000000000, 0.03515625000000000000, 0.03710937500000000000, 0.03906250000000000000, 0.04101562500000000000, 0.04296875000000000000, 0.04492187500000000000, 0.04687499999999999306, 0.04882812500000000000, 0.05078125000000000000, 0.05273437500000000000, 0.05468750000000000000, 0.05664062500000000000, 0.05859375000000000000, 0.06054687500000000000, 0.06250000000000000000, 0.06445312500000000000, 0.06640625000000000000, 0.06835937500000000000, 0.07031250000000000000, 0.07226562500000000000, 0.07421875000000000000, 0.07617187500000000000, 0.07812500000000000000, 0.08007812500000000000, 0.08203125000000000000, 0.08398437500000000000, 0.08593750000000000000, 0.08789062500000000000, 0.08984375000000000000, 0.09179687500000000000, 0.09374999999999998612, 0.09570312500000000000, 0.09765625000000000000, 0.09960937500000000000, 0.1015625000000000000, 0.1035156250000000000, 0.1054687500000000000, 0.1074218750000000000, 0.1093750000000000000, 0.1113281250000000000, 0.1132812500000000000, 0.1152343750000000000, 0.1171875000000000000, 0.1191406250000000000, 0.1210937500000000000, 0.1230468750000000000, 0.1250000000000000000, 0.1269531250000000000, 0.1289062500000000000, 0.1308593750000000000, 0.1328125000000000000, 0.1347656250000000000, 0.1367187500000000000, 0.1386718750000000000, 0.1406250000000000000, 0.1425781250000000000, 0.1445312500000000000, 0.1464843750000000000, 0.1484375000000000000, 0.1503906250000000000, 0.1523437500000000000, 0.1542968750000000000, 0.1562500000000000000, 0.1582031250000000000, 0.1601562500000000000, 0.1621093750000000000, 0.1640625000000000000, 0.1660156250000000000, 0.1679687500000000000, 0.1699218750000000000, 0.1718750000000000000, 0.1738281250000000000, 0.1757812500000000000, 0.1777343750000000000, 0.1796875000000000000, 0.1816406250000000000, 0.1835937500000000000, 0.1855468750000000000, 0.1874999999999999722, 0.1894531250000000000, 0.1914062500000000000, 0.1933593750000000000, 0.1953125000000000000, 0.1972656250000000000, 0.1992187500000000000, 0.2011718750000000000, 0.2031250000000000000, 0.2050781250000000000, 0.2070312500000000000, 0.2089843750000000000, 0.2109375000000000000, 0.2128906250000000000, 0.2148437500000000000, 0.2167968750000000000, 0.2187500000000000000, 0.2207031250000000000, 0.2226562500000000000, 0.2246093750000000000, 0.2265625000000000000, 0.2285156250000000000, 0.2304687500000000000, 0.2324218750000000000, 0.2343750000000000000, 0.2363281250000000000, 0.2382812500000000000, 0.2402343750000000000, 0.2421875000000000000, 0.2441406250000000000, 0.2460937500000000000, 0.2480468750000000000, 0.2500000000000000000, 0.2519531250000000000, 0.2539062500000000000, 0.2558593750000000000, 0.2578125000000000000, 0.2597656250000000000, 0.2617187500000000000, 0.2636718750000000000, 0.2656250000000000000, 0.2675781250000000000, 0.2695312500000000000, 0.2714843750000000000, 0.2734375000000000000, 0.2753906250000000000, 0.2773437500000000000, 0.2792968750000000000, 0.2812500000000000000, 0.2832031250000000000, 0.2851562500000000000, 0.2871093750000000000, 0.2890625000000000000, 0.2910156250000000000, 0.2929687500000000000, 0.2949218750000000000, 0.2968750000000000000, 0.2988281250000000000, 0.3007812500000000000, 0.3027343750000000000, 0.3046875000000000000, 0.3066406250000000000, 0.3085937500000000000, 0.3105468750000000000, 0.3125000000000000000, 0.3144531249999999445, 0.3164062500000000000, 0.3183593750000000000, 0.3203125000000000000, 0.3222656250000000000, 0.3242187500000000000, 0.3261718750000000000, 0.3281250000000000000, 0.3300781250000000000, 0.3320312500000000000, 0.3339843750000000000, 0.3359375000000000000, 0.3378906250000000000, 0.3398437500000000000, 0.3417968750000000000, 0.3437500000000000000, 0.3457031250000000000, 0.3476562500000000000, 0.3496093750000000000, 0.3515625000000000000, 0.3535156250000000000, 0.3554687500000000000, 0.3574218750000000000, 0.3593750000000000000, 0.3613281250000000000, 0.3632812500000000000, 0.3652343750000000000, 0.3671875000000000000, 0.3691406250000000000, 0.3710937500000000000, 0.3730468750000000000, 0.3749999999999999445, 0.3769531250000000000, 0.3789062500000000000, 0.3808593750000000000, 0.3828125000000000000, 0.3847656250000000000, 0.3867187500000000000, 0.3886718750000000000, 0.3906250000000000000, 0.3925781250000000000, 0.3945312500000000000, 0.3964843750000000000, 0.3984375000000000000, 0.4003906250000000000, 0.4023437500000000000, 0.4042968750000000000, 0.4062500000000000000, 0.4082031250000000000, 0.4101562500000000000, 0.4121093750000000000, 0.4140625000000000000, 0.4160156250000000000, 0.4179687500000000000, 0.4199218750000000000, 0.4218750000000000000, 0.4238281250000000000, 0.4257812500000000000, 0.4277343750000000000, 0.4296875000000000000, 0.4316406250000000000, 0.4335937500000000000, 0.4355468750000000555, 0.4375000000000000000, 0.4394531250000000000, 0.4414062500000000000, 0.4433593750000000000, 0.4453125000000000000, 0.4472656250000000000, 0.4492187500000000000, 0.4511718750000000000, 0.4531250000000000000, 0.4550781250000000000, 0.4570312500000000000, 0.4589843750000000000, 0.4609375000000000000, 0.4628906250000000000, 0.4648437500000000000, 0.4667968750000000000, 0.4687500000000000000, 0.4707031250000000000, 0.4726562500000000000, 0.4746093750000000000, 0.4765625000000000000, 0.4785156250000000000, 0.4804687500000000000, 0.4824218750000000000, 0.4843750000000000000, 0.4863281250000000000, 0.4882812500000000000, 0.4902343750000000000, 0.4921875000000000000, 0.4941406250000000000, 0.4960937500000000000, 0.4980468750000000000, 0.5000000000000000000, 0.5019531250000000000, 0.5039062500000000000, 0.5058593750000000000, 0.5078125000000000000, 0.5097656250000000000, 0.5117187500000000000, 0.5136718750000000000, 0.5156250000000000000, 0.5175781250000000000, 0.5195312500000000000, 0.5214843750000000000, 0.5234375000000000000, 0.5253906250000000000, 0.5273437500000000000, 0.5292968750000000000, 0.5312500000000000000, 0.5332031250000000000, 0.5351562500000000000, 0.5371093750000000000, 0.5390625000000000000, 0.5410156250000000000, 0.5429687500000000000, 0.5449218750000000000, 0.5468750000000000000, 0.5488281250000000000, 0.5507812500000000000, 0.5527343750000000000, 0.5546875000000000000, 0.5566406250000000000, 0.5585937500000000000, 0.5605468750000001110, 0.5625000000000000000, 0.5644531250000000000, 0.5664062500000000000, 0.5683593750000000000, 0.5703125000000000000, 0.5722656250000000000, 0.5742187500000000000, 0.5761718750000000000, 0.5781250000000000000, 0.5800781250000000000, 0.5820312500000000000, 0.5839843750000000000, 0.5859375000000000000, 0.5878906250000000000, 0.5898437500000000000, 0.5917968750000000000, 0.5937500000000000000, 0.5957031250000000000, 0.5976562500000000000, 0.5996093750000000000, 0.6015625000000000000, 0.6035156250000000000, 0.6054687500000000000, 0.6074218750000000000, 0.6093750000000000000, 0.6113281250000000000, 0.6132812500000000000, 0.6152343750000000000, 0.6171875000000000000, 0.6191406250000000000, 0.6210937500000000000, 0.6230468750000000000, 0.6250000000000000000, 0.6269531250000000000, 0.6289062499999998890, 0.6308593750000000000, 0.6328125000000000000, 0.6347656250000000000, 0.6367187500000000000, 0.6386718750000000000, 0.6406250000000000000, 0.6425781250000000000, 0.6445312500000000000, 0.6464843750000000000, 0.6484375000000000000, 0.6503906250000000000, 0.6523437500000000000, 0.6542968750000000000, 0.6562500000000000000, 0.6582031250000000000, 0.6601562500000000000, 0.6621093750000000000, 0.6640625000000000000, 0.6660156250000000000, 0.6679687500000000000, 0.6699218750000000000, 0.6718750000000000000, 0.6738281250000000000, 0.6757812500000000000, 0.6777343750000000000, 0.6796875000000000000, 0.6816406250000001110, 0.6835937500000000000, 0.6855468750000000000, 0.6875000000000000000, 0.6894531250000000000, 0.6914062500000000000, 0.6933593750000000000, 0.6953125000000000000, 0.6972656250000000000, 0.6992187500000000000, 0.7011718750000000000, 0.7031250000000000000, 0.7050781250000000000, 0.7070312500000000000, 0.7089843750000000000, 0.7109375000000000000, 0.7128906250000000000, 0.7148437500000000000, 0.7167968750000000000, 0.7187500000000000000, 0.7207031250000000000, 0.7226562500000000000, 0.7246093750000000000, 0.7265625000000000000, 0.7285156250000000000, 0.7304687500000000000, 0.7324218750000000000, 0.7343750000000000000, 0.7363281250000000000, 0.7382812500000000000, 0.7402343750000000000, 0.7421875000000000000, 0.7441406250000000000, 0.7460937500000000000, 0.7480468750000000000, 0.7499999999999998890, 0.7519531250000000000, 0.7539062500000000000, 0.7558593750000000000, 0.7578125000000000000, 0.7597656250000000000, 0.7617187500000000000, 0.7636718750000000000, 0.7656250000000000000, 0.7675781250000000000, 0.7695312500000000000, 0.7714843750000000000, 0.7734375000000000000, 0.7753906250000000000, 0.7773437500000000000, 0.7792968750000000000, 0.7812500000000000000, 0.7832031250000000000, 0.7851562500000000000, 0.7871093750000000000, 0.7890625000000000000, 0.7910156250000000000, 0.7929687500000000000, 0.7949218750000000000, 0.7968750000000000000, 0.7988281250000000000, 0.8007812500000000000, 0.8027343750000000000, 0.8046875000000000000, 0.8066406250000000000, 0.8085937500000000000, 0.8105468750000000000, 0.8125000000000000000, 0.8144531250000000000, 0.8164062500000000000, 0.8183593749999998890, 0.8203125000000000000, 0.8222656250000000000, 0.8242187500000000000, 0.8261718750000000000, 0.8281250000000000000, 0.8300781250000000000, 0.8320312500000000000, 0.8339843750000000000, 0.8359375000000000000, 0.8378906250000000000, 0.8398437500000000000, 0.8417968750000000000, 0.8437500000000000000, 0.8457031250000000000, 0.8476562500000000000, 0.8496093750000000000, 0.8515625000000000000, 0.8535156250000000000, 0.8554687500000000000, 0.8574218750000000000, 0.8593750000000000000, 0.8613281250000000000, 0.8632812500000000000, 0.8652343750000000000, 0.8671875000000000000, 0.8691406250000000000, 0.8710937500000001110, 0.8730468750000000000, 0.8750000000000000000, 0.8769531250000000000, 0.8789062500000000000, 0.8808593750000000000, 0.8828125000000000000, 0.8847656250000000000, 0.8867187500000000000, 0.8886718750000000000, 0.8906250000000000000, 0.8925781250000000000, 0.8945312500000000000, 0.8964843750000000000, 0.8984375000000000000, 0.9003906250000000000, 0.9023437500000000000, 0.9042968750000000000, 0.9062500000000000000, 0.9082031250000000000, 0.9101562500000000000, 0.9121093750000000000, 0.9140625000000000000, 0.9160156250000000000, 0.9179687500000000000, 0.9199218750000000000, 0.9218750000000000000, 0.9238281250000000000, 0.9257812500000000000, 0.9277343750000000000, 0.9296875000000000000, 0.9316406250000000000, 0.9335937500000000000, 0.9355468750000000000, 0.9375000000000000000, 0.9394531249999998890, 0.9414062500000000000, 0.9433593750000000000, 0.9453125000000000000, 0.9472656250000000000, 0.9492187500000000000, 0.9511718750000000000, 0.9531250000000000000, 0.9550781250000000000, 0.9570312500000000000, 0.9589843750000000000, 0.9609375000000000000, 0.9628906250000000000, 0.9648437500000000000, 0.9667968750000000000, 0.9687500000000000000, 0.9707031250000000000, 0.9726562500000000000, 0.9733142789544542151 ),
 .UNSPECIFIED. ) 
 CURVE ( )  GEOMETRIC_REPRESENTATION_ITEM ( )  RATIONAL_B_SPLINE_CURVE ( ( 1.000000000000000000, 0.9807852804032304306, 1.000000000000000000, 0.9807852804032304306, 1.000000000000000000, 0.9807852804032304306, 1.000000000000000000, 0.9807852804032304306, 1.000000000000000000, 0.9807852804032304306, 1.000000000000000000, 0.9807852804032304306, 1.000000000000000000, 0.9807852804032304306, 1.000000000000000000, 0.9807852804032304306, 1.000000000000000000, 0.9807852804032304306, 1.000000000000000000, 0.9807852804032304306, 1.000000000000000000, 0.9807852804032304306, 1.000000000000000000, 0.9807852804032304306, 1.000000000000000000, 0.9807852804032304306, 1.000000000000000000, 0.9807852804032304306, 1.000000000000000000, 0.9807852804032304306, 1.000000000000000000, 0.9807852804032304306, 1.000000000000000000, 0.9807852804032304306, 1.000000000000000000, 0.9807852804032304306, 1.000000000000000000, 0.9807852804032304306, 1.000000000000000000, 0.9807852804032304306, 1.000000000000000000, 0.9807852804032304306, 1.000000000000000000, 0.9807852804032304306, 1.000000000000000000, 0.9807852804032304306, 1.000000000000000000, 0.9807852804032304306, 1.000000000000000000, 0.9807852804032304306, 1.000000000000000000, 0.9807852804032304306, 1.000000000000000000, 0.9807852804032304306, 1.000000000000000000, 0.9807852804032304306, 1.000000000000000000, 0.9807852804032304306, 1.000000000000000000, 0.9807852804032304306, 1.000000000000000000, 0.9807852804032304306, 1.000000000000000000, 0.9807852804032304306, 1.000000000000000000, 0.9807852804032304306, 1.000000000000000000, 0.9807852804032304306, 1.000000000000000000, 0.9807852804032304306, 1.000000000000000000, 0.9807852804032304306, 1.000000000000000000, 0.9807852804032304306, 1.000000000000000000, 0.9807852804032304306, 1.000000000000000000, 0.9807852804032304306, 1.000000000000000000, 0.9807852804032304306, 1.000000000000000000, 0.9807852804032304306, 1.000000000000000000, 0.9807852804032304306, 1.000000000000000000, 0.9807852804032304306, 1.000000000000000000, 0.9807852804032304306, 1.000000000000000000, 0.9807852804032304306, 1.000000000000000000, 0.9807852804032304306, 1.000000000000000000, 0.9807852804032304306, 1.000000000000000000, 0.9807852804032304306, 1.000000000000000000, 0.9807852804032304306, 1.000000000000000000, 0.9807852804032304306, 1.000000000000000000, 0.9807852804032304306, 1.000000000000000000, 0.9807852804032304306, 1.000000000000000000, 0.9807852804032304306, 1.000000000000000000, 0.9807852804032304306, 1.000000000000000000, 0.9807852804032304306, 1.000000000000000000, 0.9807852804032304306, 1.000000000000000000, 0.9807852804032304306, 1.000000000000000000, 0.9807852804032304306, 1.000000000000000000, 0.9807852804032304306, 1.000000000000000000, 0.9807852804032304306, 1.000000000000000000, 0.9807852804032304306, 1.000000000000000000, 0.9807852804032304306, 1.000000000000000000, 0.9807852804032304306, 1.000000000000000000, 0.9807852804032304306, 1.000000000000000000, 0.9807852804032304306, 1.000000000000000000, 0.9807852804032304306, 1.000000000000000000, 0.9807852804032304306, 1.000000000000000000, 0.9807852804032304306, 1.000000000000000000, 0.9807852804032304306, 1.000000000000000000, 0.9807852804032304306, 1.000000000000000000, 0.9807852804032304306, 1.000000000000000000, 0.9807852804032304306, 1.000000000000000000, 0.9807852804032304306, 1.000000000000000000, 0.9807852804032304306, 1.000000000000000000, 0.9807852804032304306, 1.000000000000000000, 0.9807852804032304306, 1.000000000000000000, 0.9807852804032304306, 1.000000000000000000, 0.9807852804032304306, 1.000000000000000000, 0.9807852804032304306, 1.000000000000000000, 0.9807852804032304306, 1.000000000000000000, 0.9807852804032304306, 1.000000000000000000, 0.9807852804032304306, 1.000000000000000000, 0.9807852804032304306, 1.000000000000000000, 0.9807852804032304306, 1.000000000000000000, 0.9807852804032304306, 1.000000000000000000, 0.9807852804032304306, 1.000000000000000000, 0.9807852804032304306, 1.000000000000000000, 0.9807852804032304306, 1.000000000000000000, 0.9807852804032304306, 1.000000000000000000, 0.9807852804032304306, 1.000000000000000000, 0.9807852804032304306, 1.000000000000000000, 0.9807852804032304306, 1.000000000000000000, 0.9807852804032304306, 1.000000000000000000, 0.9807852804032304306, 1.000000000000000000, 0.9807852804032304306, 1.000000000000000000, 0.9807852804032304306, 1.000000000000000000, 0.9807852804032304306, 1.000000000000000000, 0.9807852804032304306, 1.000000000000000000, 0.9807852804032304306, 1.000000000000000000, 0.9807852804032304306, 1.000000000000000000, 0.9807852804032304306, 1.000000000000000000, 0.9807852804032304306, 1.000000000000000000, 0.9807852804032304306, 1.000000000000000000, 0.9807852804032304306, 1.000000000000000000, 0.9807852804032304306, 1.000000000000000000, 0.9807852804032304306, 1.000000000000000000, 0.9807852804032304306, 1.000000000000000000, 0.9807852804032304306, 1.000000000000000000, 0.9807852804032304306, 1.000000000000000000, 0.9807852804032304306, 1.000000000000000000, 0.9807852804032304306, 1.000000000000000000, 0.9807852804032304306, 1.000000000000000000, 0.9807852804032304306, 1.000000000000000000, 0.9807852804032304306, 1.000000000000000000, 0.9807852804032304306, 1.000000000000000000, 0.9807852804032304306, 1.000000000000000000, 0.9807852804032304306, 1.000000000000000000, 0.9807852804032304306, 1.000000000000000000, 0.9807852804032304306, 1.000000000000000000, 0.9807852804032304306, 1.000000000000000000, 0.9807852804032304306, 1.000000000000000000, 0.9807852804032304306, 1.000000000000000000, 0.9807852804032304306, 1.000000000000000000, 0.9807852804032304306, 1.000000000000000000, 0.9807852804032304306, 1.000000000000000000, 0.9807852804032304306, 1.000000000000000000, 0.9807852804032304306, 1.000000000000000000, 0.9807852804032304306, 1.000000000000000000, 0.9807852804032304306, 1.000000000000000000, 0.9807852804032304306, 1.000000000000000000, 0.9807852804032304306, 1.000000000000000000, 0.9807852804032304306, 1.000000000000000000, 0.9807852804032304306, 1.000000000000000000, 0.9807852804032304306, 1.000000000000000000, 0.9807852804032304306, 1.000000000000000000, 0.9807852804032304306, 1.000000000000000000, 0.9807852804032304306, 1.000000000000000000, 0.9807852804032304306, 1.000000000000000000, 0.9807852804032304306, 1.000000000000000000, 0.9807852804032304306, 1.000000000000000000, 0.9807852804032304306, 1.000000000000000000, 0.9807852804032304306, 1.000000000000000000, 0.9807852804032304306, 1.000000000000000000, 0.9807852804032304306, 1.000000000000000000, 0.9807852804032304306, 1.000000000000000000, 0.9807852804032304306, 1.000000000000000000, 0.9807852804032304306, 1.000000000000000000, 0.9807852804032304306, 1.000000000000000000, 0.9807852804032304306, 1.000000000000000000, 0.9807852804032304306, 1.000000000000000000, 0.9807852804032304306, 1.000000000000000000, 0.9807852804032304306, 1.000000000000000000, 0.9807852804032304306, 1.000000000000000000, 0.9807852804032304306, 1.000000000000000000, 0.9807852804032304306, 1.000000000000000000, 0.9807852804032304306, 1.000000000000000000, 0.9807852804032304306, 1.000000000000000000, 0.9807852804032304306, 1.000000000000000000, 0.9807852804032304306, 1.000000000000000000, 0.9807852804032304306, 1.000000000000000000, 0.9807852804032304306, 1.000000000000000000, 0.9807852804032304306, 1.000000000000000000, 0.9807852804032304306, 1.000000000000000000, 0.9807852804032304306, 1.000000000000000000, 0.9807852804032304306, 1.000000000000000000, 0.9807852804032304306, 1.000000000000000000, 0.9807852804032304306, 1.000000000000000000, 0.9807852804032304306, 1.000000000000000000, 0.9807852804032304306, 1.000000000000000000, 0.9807852804032304306, 1.000000000000000000, 0.9807852804032304306, 1.000000000000000000, 0.9807852804032304306, 1.000000000000000000, 0.9807852804032304306, 1.000000000000000000, 0.9807852804032304306, 1.000000000000000000, 0.9807852804032304306, 1.000000000000000000, 0.9807852804032304306, 1.000000000000000000, 0.9807852804032304306, 1.000000000000000000, 0.9807852804032304306, 1.000000000000000000, 0.9807852804032304306, 1.000000000000000000, 0.9807852804032304306, 1.000000000000000000, 0.9807852804032304306, 1.000000000000000000, 0.9807852804032304306, 1.000000000000000000, 0.9807852804032304306, 1.000000000000000000, 0.9807852804032304306, 1.000000000000000000, 0.9807852804032304306, 1.000000000000000000, 0.9807852804032304306, 1.000000000000000000, 0.9807852804032304306, 1.000000000000000000, 0.9807852804032304306, 1.000000000000000000, 0.9807852804032304306, 1.000000000000000000, 0.9807852804032304306, 1.000000000000000000, 0.9807852804032304306, 1.000000000000000000, 0.9807852804032304306, 1.000000000000000000, 0.9807852804032304306, 1.000000000000000000, 0.9807852804032304306, 1.000000000000000000, 0.9807852804032304306, 1.000000000000000000, 0.9807852804032304306, 1.000000000000000000, 0.9807852804032304306, 1.000000000000000000, 0.9807852804032304306, 1.000000000000000000, 0.9807852804032304306, 1.000000000000000000, 0.9807852804032304306, 1.000000000000000000, 0.9807852804032304306, 1.000000000000000000, 0.9807852804032304306, 1.000000000000000000, 0.9807852804032304306, 1.000000000000000000, 0.9807852804032304306, 1.000000000000000000, 0.9807852804032304306, 1.000000000000000000, 0.9807852804032304306, 1.000000000000000000, 0.9807852804032304306, 1.000000000000000000, 0.9807852804032304306, 1.000000000000000000, 0.9807852804032304306, 1.000000000000000000, 0.9807852804032304306, 1.000000000000000000, 0.9807852804032304306, 1.000000000000000000, 0.9807852804032304306, 1.000000000000000000, 0.9807852804032304306, 1.000000000000000000, 0.9807852804032304306, 1.000000000000000000, 0.9807852804032304306, 1.000000000000000000, 0.9807852804032304306, 1.000000000000000000, 0.9807852804032304306, 1.000000000000000000, 0.9807852804032304306, 1.000000000000000000, 0.9807852804032304306, 1.000000000000000000, 0.9807852804032304306, 1.000000000000000000, 0.9807852804032304306, 1.000000000000000000, 0.9807852804032304306, 1.000000000000000000, 0.9807852804032304306, 1.000000000000000000, 0.9807852804032304306, 1.000000000000000000, 0.9807852804032304306, 1.000000000000000000, 0.9807852804032304306, 1.000000000000000000, 0.9807852804032304306, 1.000000000000000000, 0.9807852804032304306, 1.000000000000000000, 0.9807852804032304306, 1.000000000000000000, 0.9807852804032304306, 1.000000000000000000, 0.9807852804032304306, 1.000000000000000000, 0.9807852804032304306, 1.000000000000000000, 0.9807852804032304306, 1.000000000000000000, 0.9807852804032304306, 1.000000000000000000, 0.9807852804032304306, 1.000000000000000000, 0.9807852804032304306, 1.000000000000000000, 0.9807852804032304306, 1.000000000000000000, 0.9807852804032304306, 1.000000000000000000, 0.9807852804032304306, 1.000000000000000000, 0.9807852804032304306, 1.000000000000000000, 0.9807852804032304306, 1.000000000000000000, 0.9807852804032304306, 1.000000000000000000, 0.9807852804032304306, 1.000000000000000000, 0.9807852804032304306, 1.000000000000000000, 0.9807852804032304306, 1.000000000000000000, 0.9807852804032304306, 1.000000000000000000, 0.9807852804032304306, 1.000000000000000000, 0.9807852804032304306, 1.000000000000000000, 0.9807852804032304306, 1.000000000000000000, 0.9807852804032304306, 1.000000000000000000, 0.9807852804032304306, 1.000000000000000000, 0.9807852804032304306, 1.000000000000000000, 0.9807852804032304306, 1.000000000000000000, 0.9807852804032304306, 1.000000000000000000, 0.9807852804032304306, 1.000000000000000000, 0.9807852804032304306, 1.000000000000000000, 0.9807852804032304306, 1.000000000000000000, 0.9807852804032304306, 1.000000000000000000, 0.9807852804032304306, 1.000000000000000000, 0.9807852804032304306, 1.000000000000000000, 0.9807852804032304306, 1.000000000000000000, 0.9807852804032304306, 1.000000000000000000, 0.9807852804032304306, 1.000000000000000000, 0.9807852804032304306, 1.000000000000000000, 0.9807852804032304306, 1.000000000000000000, 0.9807852804032304306, 1.000000000000000000, 0.9807852804032304306, 1.000000000000000000, 0.9807852804032304306, 1.000000000000000000, 0.9807852804032304306, 1.000000000000000000, 0.9807852804032304306, 1.000000000000000000, 0.9807852804032304306, 1.000000000000000000, 0.9807852804032304306, 1.000000000000000000, 0.9807852804032304306, 1.000000000000000000, 0.9807852804032304306, 1.000000000000000000, 0.9807852804032304306, 1.000000000000000000, 0.9807852804032304306, 1.000000000000000000, 0.9807852804032304306, 1.000000000000000000, 0.9807852804032304306, 1.000000000000000000, 0.9807852804032304306, 1.000000000000000000, 0.9807852804032304306, 1.000000000000000000, 0.9807852804032304306, 1.000000000000000000, 0.9807852804032304306, 1.000000000000000000, 0.9807852804032304306, 1.000000000000000000, 0.9807852804032304306, 1.000000000000000000, 0.9807852804032304306, 1.000000000000000000, 0.9807852804032304306, 1.000000000000000000, 0.9807852804032304306, 1.000000000000000000, 0.9807852804032304306, 1.000000000000000000, 0.9807852804032304306, 1.000000000000000000, 0.9807852804032304306, 1.000000000000000000, 0.9807852804032304306, 1.000000000000000000, 0.9807852804032304306, 1.000000000000000000, 0.9807852804032304306, 1.000000000000000000, 0.9807852804032304306, 1.000000000000000000, 0.9807852804032304306, 1.000000000000000000, 0.9807852804032304306, 1.000000000000000000, 0.9807852804032304306, 1.000000000000000000, 0.9807852804032304306, 1.000000000000000000, 0.9807852804032304306, 1.000000000000000000, 0.9807852804032304306, 1.000000000000000000, 0.9807852804032304306, 1.000000000000000000, 0.9807852804032304306, 1.000000000000000000, 0.9807852804032304306, 1.000000000000000000, 0.9807852804032304306, 1.000000000000000000, 0.9807852804032304306, 1.000000000000000000, 0.9807852804032304306, 1.000000000000000000, 0.9807852804032304306, 1.000000000000000000, 0.9807852804032304306, 1.000000000000000000, 0.9807852804032304306, 1.000000000000000000, 0.9807852804032304306, 1.000000000000000000, 0.9807852804032304306, 1.000000000000000000, 0.9807852804032304306, 1.000000000000000000, 0.9807852804032304306, 1.000000000000000000, 0.9807852804032304306, 1.000000000000000000, 0.9807852804032304306, 1.000000000000000000, 0.9807852804032304306, 1.000000000000000000, 0.9807852804032304306, 1.000000000000000000, 0.9807852804032304306, 1.000000000000000000, 0.9807852804032304306, 1.000000000000000000, 0.9807852804032304306, 1.000000000000000000, 0.9807852804032304306, 1.000000000000000000, 0.9807852804032304306, 1.000000000000000000, 0.9807852804032304306, 1.000000000000000000, 0.9807852804032304306, 1.000000000000000000, 0.9807852804032304306, 1.000000000000000000, 0.9807852804032304306, 1.000000000000000000, 0.9807852804032304306, 1.000000000000000000, 0.9807852804032304306, 1.000000000000000000, 0.9807852804032304306, 1.000000000000000000, 0.9807852804032304306, 1.000000000000000000, 0.9807852804032304306, 1.000000000000000000, 0.9807852804032304306, 1.000000000000000000, 0.9807852804032304306, 1.000000000000000000, 0.9807852804032304306, 1.000000000000000000, 0.9807852804032304306, 1.000000000000000000, 0.9807852804032304306, 1.000000000000000000, 0.9807852804032304306, 1.000000000000000000, 0.9807852804032304306, 1.000000000000000000, 0.9807852804032304306, 1.000000000000000000, 0.9807852804032304306, 1.000000000000000000, 0.9807852804032304306, 1.000000000000000000, 0.9807852804032304306, 1.000000000000000000, 0.9807852804032304306, 1.000000000000000000, 0.9807852804032304306, 1.000000000000000000, 0.9807852804032304306, 1.000000000000000000, 0.9807852804032304306, 1.000000000000000000, 0.9807852804032304306, 1.000000000000000000, 0.9807852804032304306, 1.000000000000000000, 0.9807852804032304306, 1.000000000000000000, 0.9807852804032304306, 1.000000000000000000, 0.9807852804032304306, 1.000000000000000000, 0.9807852804032304306, 1.000000000000000000, 0.9807852804032304306, 1.000000000000000000, 0.9807852804032304306, 1.000000000000000000, 0.9807852804032304306, 1.000000000000000000, 0.9807852804032304306, 1.000000000000000000, 0.9807852804032304306, 1.000000000000000000, 0.9807852804032304306, 1.000000000000000000, 0.9807852804032304306, 1.000000000000000000, 0.9807852804032304306, 1.000000000000000000, 0.9807852804032304306, 1.000000000000000000, 0.9807852804032304306, 1.000000000000000000, 0.9807852804032304306, 1.000000000000000000, 0.9807852804032304306, 1.000000000000000000, 0.9807852804032304306, 1.000000000000000000, 0.9807852804032304306, 1.000000000000000000, 0.9807852804032304306, 1.000000000000000000, 0.9807852804032304306, 1.000000000000000000, 0.9807852804032304306, 1.000000000000000000, 0.9807852804032304306, 1.000000000000000000, 0.9807852804032304306, 1.000000000000000000, 0.9807852804032304306, 1.000000000000000000, 0.9807852804032304306, 1.000000000000000000, 0.9807852804032304306, 1.000000000000000000, 0.9807852804032304306, 1.000000000000000000, 0.9807852804032304306, 1.000000000000000000, 0.9807852804032304306, 1.000000000000000000, 0.9807852804032304306, 1.000000000000000000, 0.9807852804032304306, 1.000000000000000000, 0.9807852804032304306, 1.000000000000000000, 0.9807852804032304306, 1.000000000000000000, 0.9807852804032304306, 1.000000000000000000, 0.9807852804032304306, 1.000000000000000000, 0.9807852804032304306, 1.000000000000000000, 0.9807852804032304306, 1.000000000000000000, 0.9807852804032304306, 1.000000000000000000, 0.9807852804032304306, 1.000000000000000000, 0.9807852804032304306, 1.000000000000000000, 0.9807852804032304306, 1.000000000000000000, 0.9807852804032304306, 1.000000000000000000, 0.9807852804032304306, 1.000000000000000000, 0.9807852804032304306, 1.000000000000000000, 0.9807852804032304306, 1.000000000000000000, 0.9807852804032304306, 1.000000000000000000, 0.9807852804032304306, 1.000000000000000000, 0.9807852804032304306, 1.000000000000000000, 0.9807852804032304306, 1.000000000000000000, 0.9807852804032304306, 1.000000000000000000, 0.9807852804032304306, 1.000000000000000000, 0.9807852804032304306, 1.000000000000000000, 0.9807852804032304306, 1.000000000000000000, 0.9807852804032304306, 1.000000000000000000, 0.9807852804032304306, 1.000000000000000000, 0.9807852804032304306, 1.000000000000000000, 0.9807852804032304306, 1.000000000000000000, 0.9807852804032304306, 1.000000000000000000, 0.9807852804032304306, 1.000000000000000000, 0.9807852804032304306, 1.000000000000000000, 0.9807852804032304306, 1.000000000000000000, 0.9807852804032304306, 1.000000000000000000, 0.9807852804032304306, 1.000000000000000000, 0.9807852804032304306, 1.000000000000000000, 0.9807852804032304306, 1.000000000000000000, 0.9807852804032304306, 1.000000000000000000, 0.9807852804032304306, 1.000000000000000000, 0.9807852804032304306, 1.000000000000000000, 0.9807852804032304306, 1.000000000000000000, 0.9807852804032304306, 1.000000000000000000, 0.9807852804032304306, 1.000000000000000000, 0.9807852804032304306, 1.000000000000000000, 0.9807852804032304306, 1.000000000000000000, 0.9807852804032304306, 1.000000000000000000, 0.9807852804032304306, 1.000000000000000000, 0.9807852804032304306, 1.000000000000000000, 0.9807852804032304306, 1.000000000000000000, 0.9807852804032304306, 1.000000000000000000, 0.9807852804032304306, 1.000000000000000000, 0.9807852804032304306, 1.000000000000000000, 0.9807852804032304306, 1.000000000000000000, 0.9807852804032304306, 1.000000000000000000, 0.9807852804032304306, 1.000000000000000000, 0.9807852804032304306, 1.000000000000000000, 0.9807852804032304306, 1.000000000000000000, 0.9807852804032304306, 1.000000000000000000, 0.9807852804032304306, 1.000000000000000000, 0.9807852804032304306, 1.000000000000000000, 0.9807852804032304306, 1.000000000000000000, 0.9807852804032304306, 1.000000000000000000, 0.9807852804032304306, 1.000000000000000000, 0.9807852804032304306, 1.000000000000000000, 0.9807852804032304306, 1.000000000000000000, 0.9807852804032304306, 1.000000000000000000, 0.9807852804032304306, 1.000000000000000000, 0.9807852804032304306, 1.000000000000000000, 0.9807852804032304306, 1.000000000000000000, 0.9807852804032304306, 1.000000000000000000, 0.9807852804032304306, 1.000000000000000000, 0.9807852804032304306, 1.000000000000000000, 0.9807852804032304306, 1.000000000000000000, 0.9807852804032304306, 1.000000000000000000, 0.9807852804032304306, 1.000000000000000000, 0.9807852804032304306, 1.000000000000000000, 0.9807852804032304306, 1.000000000000000000, 0.9807852804032304306, 1.000000000000000000, 0.9807852804032304306, 1.000000000000000000, 0.9807852804032304306, 1.000000000000000000, 0.9807852804032304306, 1.000000000000000000, 0.9807852804032304306, 1.000000000000000000, 0.9807852804032304306, 1.000000000000000000, 0.9807852804032304306, 1.000000000000000000, 0.9807852804032304306, 1.000000000000000000, 0.9807852804032304306, 1.000000000000000000, 0.9807852804032304306, 1.000000000000000000, 0.9807852804032304306, 1.000000000000000000, 0.9807852804032304306, 1.000000000000000000, 0.9807852804032304306, 1.000000000000000000, 0.9807852804032304306, 1.000000000000000000, 0.9807852804032304306, 1.000000000000000000, 0.9807852804032304306, 1.000000000000000000, 0.9807852804032304306, 1.000000000000000000, 0.9807852804032304306, 1.000000000000000000, 0.9807852804032304306, 1.000000000000000000, 0.9807852804032304306, 1.000000000000000000, 0.9807852804032304306, 1.000000000000000000, 0.9807852804032304306, 1.000000000000000000, 0.9807852804032304306, 1.000000000000000000, 0.9807852804032304306, 1.000000000000000000, 0.9807852804032304306, 1.000000000000000000, 0.9807852804032304306, 1.000000000000000000, 0.9807852804032304306, 1.000000000000000000, 0.9807852804032304306, 1.000000000000000000, 0.9807852804032304306, 1.000000000000000000, 0.9807852804032304306, 1.000000000000000000, 0.9807852804032304306, 1.000000000000000000, 0.9807852804032304306, 1.000000000000000000, 0.9807852804032304306, 1.000000000000000000, 0.9807852804032304306, 1.000000000000000000, 0.9807852804032304306, 1.000000000000000000, 0.9807852804032304306, 1.000000000000000000, 0.9807852804032304306, 1.000000000000000000, 0.9807852804032304306, 1.000000000000000000, 0.9807852804032304306, 1.000000000000000000, 0.9807852804032304306, 1.000000000000000000, 0.9807852804032304306, 1.000000000000000000, 0.9807852804032304306, 1.000000000000000000, 0.9807852804032304306, 1.000000000000000000, 0.9807852804032304306, 1.000000000000000000, 0.9807852804032304306, 1.000000000000000000, 0.9935263529746467537, 0.9914147894652987070 ) ) 
 REPRESENTATION_ITEM ( '' )  );
#187 = CARTESIAN_POINT ( 'NONE',  ( -35.09675569278796559, 521.9948905683720568, -15.47720386886985544 ) ) ;
#188 = ORIENTED_EDGE ( 'NONE', *, *, #12536, .T. ) ;
#189 = CARTESIAN_POINT ( 'NONE',  ( -28.68588794268874054, 573.2448905601785327, 0.000000000000000000 ) ) ;
#190 = CARTESIAN_POINT ( 'NONE',  ( -45.43829269268871940, 484.1823905683720000, 3.332260488124734632 ) ) ;
#191 = ORIENTED_EDGE ( 'NONE', *, *, #19278, .F. ) ;
#192 = CARTESIAN_POINT ( 'NONE',  ( -22.27502019258949417, 496.9948905683720568, 15.47720386886985189 ) ) ;
#193 = CARTESIAN_POINT ( 'NONE',  ( -18.46114582419561856, 45.97303840584705625, -48.53623208051946136 ) ) ;
#194 = CARTESIAN_POINT ( 'NONE',  ( -28.68588794268871922, 414.4948905765656377, 19.99999999999999289 ) ) ;
#195 = CARTESIAN_POINT ( 'NONE',  ( 71.32175588950862277, 75.31183677523708297, 40.00000000000000000 ) ) ;
#196 = CARTESIAN_POINT ( 'NONE',  ( -28.68588794268870856, 329.7448905601784759, 19.99999999999999289 ) ) ;
#197 = DIRECTION ( 'NONE',  ( 0.000000000000000000, 0.000000000000000000, 1.000000000000000000 ) ) ;
#198 = CARTESIAN_POINT ( 'NONE',  ( 1.395063264127832658E-15, -5.788408252967908396, -2.974182810908600150 ) ) ;
#199 = EDGE_CURVE ( 'NONE', #182, #19453, #6902, .T. ) ;
#200 = DIRECTION ( 'NONE',  ( 0.000000000000000000, 0.000000000000000000, -1.000000000000000000 ) ) ;
#201 = CARTESIAN_POINT ( 'NONE',  ( -43.20715004130836689, 201.8397834041948613, -3.766744768033091884 ) ) ;
#202 = CARTESIAN_POINT ( 'NONE',  ( -19.19641293061497933, 291.9323905683720568, -14.20200298773971603 ) ) ;
#203 = CARTESIAN_POINT ( 'NONE',  ( -36.33955658999053639, 529.1198905601785327, 18.47759065022572500 ) ) ;
#204 = AXIS2_PLACEMENT_3D ( 'NONE', #20322, #335, #6901 ) ;
#205 = CARTESIAN_POINT ( 'NONE',  ( -8.685887942688710339, 262.2448905601784759, -2.449293598294705724E-15 ) ) ;
#206 = CARTESIAN_POINT ( 'NONE',  ( -31.47597222270714212, 49.78415940255306538, -49.52648848774079937 ) ) ;
#207 = CARTESIAN_POINT ( 'NONE',  ( -13.20868407381885135, 280.9948905683720000, -6.410867750099233042 ) ) ;
#208 = CARTESIAN_POINT ( 'NONE',  ( -28.68588794268873698, 534.7448905601785327, -19.99999999999999289 ) ) ;
#209 = CARTESIAN_POINT ( 'NONE',  ( -42.88789093042844769, 496.3073905683721136, 9.489475012073734561 ) ) ;
#210 = EDGE_CURVE ( 'NONE', #6677, #9516, #4265, .T. ) ;
#211 = FACE_OUTER_BOUND ( 'NONE', #7331, .T. ) ;
#212 = ORIENTED_EDGE ( 'NONE', *, *, #19326, .T. ) ;
#213 = CARTESIAN_POINT ( 'NONE',  ( -28.68588794268872988, 462.8698905683720000, -16.75240474999999307 ) ) ;
#214 = DIRECTION ( 'NONE',  ( -1.000000000000000000, -0.000000000000000000, -0.000000000000000000 ) ) ;
#215 = CARTESIAN_POINT ( 'NONE',  ( -14.48388495494898720, 267.9323905683720568, 9.489475012073732785 ) ) ;
#216 = ORIENTED_EDGE ( 'NONE', *, *, #18810, .T. ) ;
#217 = CARTESIAN_POINT ( 'NONE',  ( -8.685887942688742314, 573.2448905601785327, 2.449293598294706119E-15 ) ) ;
#218 = CARTESIAN_POINT ( 'NONE',  ( -38.17536295476244135, 233.8073905683720284, -14.20200298773971426 ) ) ;
#219 = EDGE_CURVE ( 'NONE', #12803, #14751, #2645, .T. ) ;
#220 = CARTESIAN_POINT ( 'NONE',  ( -48.68588794268869435, 251.6823905765656093, -3.978247347593158345 ) ) ;
#221 = CARTESIAN_POINT ( 'NONE',  ( -21.03221929538690205, 310.3698905601784759, 18.47759065022572500 ) ) ;
#222 = CARTESIAN_POINT ( 'NONE',  ( -28.68588794268870146, 234.7448905601785043, -19.99999999999999289 ) ) ;
#223 = CARTESIAN_POINT ( 'NONE',  ( -8.685887942688726326, 412.2448905601784759, -2.449293598294705724E-15 ) ) ;
#224 = CARTESIAN_POINT ( 'NONE',  ( -11.93348319268870839, 258.8698905683720000, -2.051577885510841163E-15 ) ) ;
#225 = CARTESIAN_POINT ( 'NONE',  ( -40.53162694259543741, 354.1198905683720568, -11.84573899990672707 ) ) ;
#226 = CARTESIAN_POINT ( 'NONE',  ( -48.68588794268865882, 506.9323905601784759, -3.978247347593317773 ) ) ;
#227 = CARTESIAN_POINT ( 'NONE',  ( 60.03793209889851568, 30.52886280891152282, -131.1729372809869005 ) ) ;
#228 = CARTESIAN_POINT ( 'NONE',  ( -25.35362745456398770, 416.6823905683720568, 16.75240474999998952 ) ) ;
#229 = CARTESIAN_POINT ( 'NONE',  ( 5.674999999999999822, 3.752776749732560368, -6.499999999999999112 ) ) ;
#230 = ORIENTED_EDGE ( 'NONE', *, *, #2551, .F. ) ;
#231 = CARTESIAN_POINT ( 'NONE',  ( -36.33955658999051508, 415.3698905601784759, -18.47759065022572855 ) ) ;
#232 = VERTEX_POINT ( 'NONE', #18752 ) ;
#233 = ORIENTED_EDGE ( 'NONE', *, *, #12800, .T. ) ;
#234 = ORIENTED_EDGE ( 'NONE', *, *, #8898, .F. ) ;
#235 = CARTESIAN_POINT ( 'NONE',  ( -25.35362745456401257, 532.5573905683720568, -16.75240474999999307 ) ) ;
#236 = CARTESIAN_POINT ( 'NONE',  ( -28.68588794268870856, 304.7448905601785327, -19.99999999999999289 ) ) ;
#237 = CARTESIAN_POINT ( 'NONE',  ( -43.60140439023966508, 209.8858117899327169, -1.618481238659646326 ) ) ;
#238 = ORIENTED_EDGE ( 'NONE', *, *, #8071, .F. ) ;
#239 = CARTESIAN_POINT ( 'NONE',  ( -45.43829269268870519, 325.0573905683719431, -3.332260488124726638 ) ) ;
#240 = ORIENTED_EDGE ( 'NONE', *, *, #13467, .F. ) ;
#241 = CARTESIAN_POINT ( 'NONE',  ( -38.17536295476245556, 372.3073905683721136, -14.20200298773971426 ) ) ;
#242 = CARTESIAN_POINT ( 'NONE',  ( -40.53162694259543741, 372.6198905683720000, -11.84573899990672707 ) ) ;
#243 = VECTOR ( 'NONE', #20484, 1000.000000000000000 ) ;
#244 = CARTESIAN_POINT ( 'NONE',  ( -11.73070664223723902, 296.0573905765655809, 11.32908994701042005 ) ) ;
#245 = DIRECTION ( 'NONE',  ( -1.000000000000000000, 0.000000000000000000, 0.000000000000000000 ) ) ;
#246 = CARTESIAN_POINT ( 'NONE',  ( -45.43829269268869808, 263.5573905683720000, -3.332260488124726638 ) ) ;
#247 = CARTESIAN_POINT ( 'NONE',  ( -47.16347859291445133, 437.8698905601784759, 7.653668647301805628 ) ) ;
#248 = EDGE_CURVE ( 'NONE', #20201, #15177, #9669, .T. ) ;
#249 = CARTESIAN_POINT ( 'NONE',  ( -16.84014894278199392, 419.1198905683720000, 11.84573899990672530 ) ) ;
#250 = EDGE_CURVE ( 'NONE', #13614, #661, #3833, .T. ) ;
#251 = AXIS2_PLACEMENT_3D ( 'NONE', #16100, #3221, #14485 ) ;
#252 = LINE ( 'NONE', #16791, #13736 ) ;
#253 = CARTESIAN_POINT ( 'NONE',  ( -24.70764059509557597, 514.4323905601785327, -19.99999999999999289 ) ) ;
#254 = CARTESIAN_POINT ( 'NONE',  ( -28.68588794268874054, 573.2448905601785327, 0.000000000000000000 ) ) ;
#255 = CARTESIAN_POINT ( 'NONE',  ( -17.35679799567829917, 450.6823905601784759, 16.95518130045146421 ) ) ;
#256 = CARTESIAN_POINT ( 'NONE',  ( -11.93348319268871727, 320.0573905683720000, 3.332260488124728415 ) ) ;
#257 = CARTESIAN_POINT ( 'NONE',  ( -42.88789093042844769, 492.9323905683720568, -9.489475012073736337 ) ) ;
#258 = VERTEX_POINT ( 'NONE', #20385 ) ;
#259 = CARTESIAN_POINT ( 'NONE',  ( -40.01497788969914637, 458.8073905601784759, 16.95518130045146776 ) ) ;
#260 = CARTESIAN_POINT ( 'NONE',  ( -16.84014894278198327, 300.1198905683720000, -11.84573899990672707 ) ) ;
#261 = AXIS2_PLACEMENT_3D ( 'NONE', #1279, #21066, #12850 ) ;
#262 = ORIENTED_EDGE ( 'NONE', *, *, #2754, .T. ) ;
#263 = CARTESIAN_POINT ( 'NONE',  ( -48.68588794268870856, 341.9948905765656377, 0.000000000000000000 ) ) ;
#264 = VERTEX_POINT ( 'NONE', #824 ) ;
#265 = CARTESIAN_POINT ( 'NONE',  ( 158.8141120573112630, 400.5398297725602674, 5.000000000000004441 ) ) ;
#266 = CIRCLE ( 'NONE', #20628, 10.00000000000000888 ) ;
#267 = CARTESIAN_POINT ( 'NONE',  ( -35.09675569278795138, 387.2448905683720000, 15.47720386886985366 ) ) ;
#268 = FACE_OUTER_BOUND ( 'NONE', #16614, .T. ) ;
#269 = CARTESIAN_POINT ( 'NONE',  ( -28.68588794268871922, 416.3698905683720568, 16.75240474999999307 ) ) ;
#270 = CARTESIAN_POINT ( 'NONE',  ( -45.43829269268869808, 255.3698905683720000, 0.000000000000000000 ) ) ;
#271 = CARTESIAN_POINT ( 'NONE',  ( -35.09675569278795848, 425.7448905683720000, 15.47720386886985366 ) ) ;
#272 = APPLICATION_PROTOCOL_DEFINITION ( 'draft international standard', 'automotive_design', 1998, #3894 ) ;
#273 = LINE ( 'NONE', #3605, #8631 ) ;
#274 = CARTESIAN_POINT ( 'NONE',  ( -21.03221929538690915, 365.1198905765656377, 18.47759065022572500 ) ) ;
#275 = CARTESIAN_POINT ( 'NONE',  ( 18.55315245287936321, 326.0737056351150613, 0.000000000000000000 ) ) ;
#276 = DIRECTION ( 'NONE',  ( 1.000000000000000000, 0.000000000000000000, 0.000000000000000000 ) ) ;
#277 = CARTESIAN_POINT ( 'NONE',  ( -45.43829269268871229, 334.1823905683720000, 3.332260488124734632 ) ) ;
#278 = DIRECTION ( 'NONE',  ( 0.000000000000000000, 1.000000000000000000, 0.000000000000000000 ) ) ;
#279 = CARTESIAN_POINT ( 'NONE',  ( -16.84014894278200458, 481.6198905683720000, -11.84573899990672707 ) ) ;
#280 = VECTOR ( 'NONE', #18343, 1000.000000000000000 ) ;
#281 = CARTESIAN_POINT ( 'NONE',  ( 79.78925230247502043, 142.5259582928263455, -20.00000000000000355 ) ) ;
#282 = CARTESIAN_POINT ( 'NONE',  ( -21.03221929538692692, 520.3698905601785327, 18.47759065022572500 ) ) ;
#283 = CARTESIAN_POINT ( 'NONE',  ( -35.09675569278795848, 397.2448905683720568, 15.47720386886985366 ) ) ;
#284 = CARTESIAN_POINT ( 'NONE',  ( -48.68588794268886488, 262.3073905765655240, 3.978247347592742678 ) ) ;
#285 = CARTESIAN_POINT ( 'NONE',  ( -19.19641293061496512, 228.8073905683720284, 14.20200298773971426 ) ) ;
#286 = CARTESIAN_POINT ( 'NONE',  ( -13.20868407381886200, 369.4948905683720568, -6.410867750099233042 ) ) ;
#287 = ORIENTED_EDGE ( 'NONE', *, *, #20481, .T. ) ;
#288 = CARTESIAN_POINT ( 'NONE',  ( -11.93348319268874214, 529.1823905683719431, -3.332260488124732856 ) ) ;
#289 = VERTEX_POINT ( 'NONE', #7390 ) ;
#290 = CARTESIAN_POINT ( 'NONE',  ( -45.43829269268871940, 445.6823905683720000, 3.332260488124734632 ) ) ;
#291 = CARTESIAN_POINT ( 'NONE',  ( -19.19641293061500065, 527.3073905683720568, 14.20200298773971426 ) ) ;
#292 = FACE_OUTER_BOUND ( 'NONE', #157, .T. ) ;
#293 = CARTESIAN_POINT ( 'NONE',  ( -42.82802356641968089, 530.7448905765656946, -14.14213562373094746 ) ) ;
#294 = CARTESIAN_POINT ( 'NONE',  ( -28.68588794268872988, 481.3698905683720568, -16.75240474999999307 ) ) ;
#295 = ORIENTED_EDGE ( 'NONE', *, *, #7360, .T. ) ;
#296 = CARTESIAN_POINT ( 'NONE',  ( -35.09675569278797269, 505.7448905683720000, 15.47720386886985366 ) ) ;
#297 = CARTESIAN_POINT ( 'NONE',  ( -13.97728958318061565, 48.85369832438319548, -47.37148056848186428 ) ) ;
#298 = CARTESIAN_POINT ( 'NONE',  ( -45.64106924314019409, 422.9323905765656377, 11.32908994701042715 ) ) ;
#299 = DIRECTION ( 'NONE',  ( 1.000000000000000000, 0.000000000000000000, 0.000000000000000000 ) ) ;
#300 = EDGE_CURVE ( 'NONE', #14946, #18462, #14017, .T. ) ;
#301 = CARTESIAN_POINT ( 'NONE',  ( -11.73070664223723547, 247.9323905765656377, -11.32908994701042538 ) ) ;
#302 = CARTESIAN_POINT ( 'NONE',  ( -36.33955658999052218, 485.3698905601784759, -18.47759065022572855 ) ) ;
#303 = DIRECTION ( 'NONE',  ( 0.000000000000000000, -1.000000000000000000, 0.000000000000000000 ) ) ;
#304 = CARTESIAN_POINT ( 'NONE',  ( 0.000000000000000000, -5.629165124598849879, -3.250000000000003553 ) ) ;
#305 = DIRECTION ( 'NONE',  ( 0.000000000000000000, 1.000000000000000000, 0.000000000000000000 ) ) ;
#306 = CARTESIAN_POINT ( 'NONE',  ( -10.48919683876846420, 223.9102039777117170, -8.480601754011892979 ) ) ;
#307 = CARTESIAN_POINT ( 'NONE',  ( -28.68588794268870146, 287.8698905683720568, 16.75240474999999307 ) ) ;
#308 = LINE ( 'NONE', #5261, #20260 ) ;
#309 = CARTESIAN_POINT ( 'NONE',  ( -42.82802356641965247, 278.4948905601785327, 14.14213562373094923 ) ) ;
#310 = CARTESIAN_POINT ( 'NONE',  ( -28.68588794268872988, 47.23886018424757083, -49.60091809715359545 ) ) ;
#311 =( BOUNDED_CURVE ( )  B_SPLINE_CURVE ( 2, ( #7202, #2045, #13619, #18362, #8409, #6891, #16759, #18573, #15242, #5273, #3755, #1946, #8514, #15141, #15354, #8617, #13511 ),
 .UNSPECIFIED., .F., .T. ) 
 B_SPLINE_CURVE_WITH_KNOTS ( ( 3, 2, 2, 2, 2, 2, 2, 2, 3 ),
 ( 0.6093750000000002220, 0.6113281250000002220, 0.6132812500000002220, 0.6152343750000002220, 0.6171875000000002220, 0.6191406250000002220, 0.6210937500000002220, 0.6230468750000002220, 0.6250000000000002220 ),
 .UNSPECIFIED. ) 
 CURVE ( )  GEOMETRIC_REPRESENTATION_ITEM ( )  RATIONAL_B_SPLINE_CURVE ( ( 0.9999999999999977796, 0.9807852804032326510, 1.000000000000000000, 0.9807852804032304306, 1.000000000000000000, 0.9807852804032304306, 1.000000000000000000, 0.9807852804032304306, 1.000000000000000000, 0.9807852804032304306, 1.000000000000000000, 0.9807852804032304306, 1.000000000000000000, 0.9807852804032304306, 1.000000000000000000, 0.9807852804032282101, 1.000000000000002220 ) ) 
 REPRESENTATION_ITEM ( '' )  );
#312 = CARTESIAN_POINT ( 'NONE',  ( -42.88789093042842637, 294.4323905683720568, -9.489475012073736337 ) ) ;
#313 = VERTEX_POINT ( 'NONE', #1450 ) ;
#314 = CARTESIAN_POINT ( 'NONE',  ( -24.70764059509553690, 270.0573905601784759, 19.99999999999998934 ) ) ;
#315 = CARTESIAN_POINT ( 'NONE',  ( -40.53162694259545162, 496.6198905683720000, 11.84573899990672885 ) ) ;
#316 = ADVANCED_FACE ( 'NONE', ( #2968 ), #17876, .T. ) ;
#317 = ORIENTED_EDGE ( 'NONE', *, *, #11658, .T. ) ;
#318 = CARTESIAN_POINT ( 'NONE',  ( -38.17536295476246266, 466.9323905683720568, 14.20200298773971781 ) ) ;
#319 = DIRECTION ( 'NONE',  ( -0.000000000000000000, -1.000000000000000000, -0.000000000000000000 ) ) ;
#320 = CARTESIAN_POINT ( 'NONE',  ( -11.93348319268871194, 268.5573905683720568, 3.332260488124728415 ) ) ;
#321 = ORIENTED_EDGE ( 'NONE', *, *, #1301, .F. ) ;
#322 = CARTESIAN_POINT ( 'NONE',  ( -48.68588794268873698, 573.2448905601785327, 0.000000000000000000 ) ) ;
#323 = AXIS2_PLACEMENT_3D ( 'NONE', #6998, #18893, #7103 ) ;
#324 = PRODUCT_DEFINITION ( 'UNKNOWN', '', #14550, #16365 ) ;
#325 = CARTESIAN_POINT ( 'NONE',  ( -45.43829269268869808, 245.3698905683720568, 0.000000000000000000 ) ) ;
#326 = CARTESIAN_POINT ( 'NONE',  ( -32.66413529028186247, 239.8073905765656377, -19.99999999999999289 ) ) ;
#327 = CARTESIAN_POINT ( 'NONE',  ( -17.35679799567828141, 310.6823905601784759, 16.95518130045146421 ) ) ;
#328 = CARTESIAN_POINT ( 'NONE',  ( -45.64106924314017277, 226.3073905601784759, -11.32908994701042715 ) ) ;
#329 = CARTESIAN_POINT ( 'NONE',  ( -11.93348319268871194, 268.5573905683720568, 3.332260488124728415 ) ) ;
#330 = CARTESIAN_POINT ( 'NONE',  ( -32.01814843081344719, 367.5573905683721136, 16.75240474999999307 ) ) ;
#331 = EDGE_CURVE ( 'NONE', #9067, #11943, #8433, .T. ) ;
#332 = DIRECTION ( 'NONE',  ( 0.000000000000000000, -0.000000000000000000, -1.000000000000000000 ) ) ;
#333 = AXIS2_PLACEMENT_3D ( 'NONE', #2652, #9240, #18099 ) ;
#334 = CARTESIAN_POINT ( 'NONE',  ( -42.88789093042844058, 412.9323905683720000, -9.489475012073736337 ) ) ;
#335 = DIRECTION ( 'NONE',  ( -0.000000000000000000, 1.000000000000000000, -0.000000000000000000 ) ) ;
#336 = ORIENTED_EDGE ( 'NONE', *, *, #8233, .F. ) ;
#337 = CARTESIAN_POINT ( 'NONE',  ( -10.20829729246299067, 402.8698905601784759, -7.653668647301794969 ) ) ;
#338 = ADVANCED_FACE ( 'NONE', ( #9446 ), #11276, .T. ) ;
#339 = VERTEX_POINT ( 'NONE', #6303 ) ;
#340 = CARTESIAN_POINT ( 'NONE',  ( -5.251604272976662102E-16, 0.6351314446054973084, -6.500000000000000000 ) ) ;
#341 = ORIENTED_EDGE ( 'NONE', *, *, #9677, .F. ) ;
#342 = ORIENTED_EDGE ( 'NONE', *, *, #2095, .T. ) ;
#343 = CARTESIAN_POINT ( 'NONE',  ( -35.09675569278796559, 533.4948905683720568, -15.47720386886985544 ) ) ;
#344 = VECTOR ( 'NONE', #10639, 1000.000000000000000 ) ;
#345 = CARTESIAN_POINT ( 'NONE',  ( -17.35679799567828852, 283.8073905601784190, -16.95518130045146421 ) ) ;
#346 = PLANE ( 'NONE',  #8685 ) ;
#347 = ORIENTED_EDGE ( 'NONE', *, *, #16944, .T. ) ;
#348 = CARTESIAN_POINT ( 'NONE',  ( -14.48388495494899431, 329.4323905683720568, 9.489475012073731008 ) ) ;
#349 = VERTEX_POINT ( 'NONE', #11382 ) ;
#350 = CARTESIAN_POINT ( 'NONE',  ( -28.68588794268871212, 366.3698905683720568, 16.75240474999999307 ) ) ;
#351 = CARTESIAN_POINT ( 'NONE',  ( -19.19641293061498288, 360.4323905683720000, -14.20200298773971603 ) ) ;
#352 = VECTOR ( 'NONE', #18176, 1000.000000000000000 ) ;
#353 = CARTESIAN_POINT ( 'NONE',  ( -28.68588794268870501, 294.4948905765656377, 19.99999999999999289 ) ) ;
#354 = FACE_OUTER_BOUND ( 'NONE', #1771, .T. ) ;
#355 = CARTESIAN_POINT ( 'NONE',  ( -19.19641293061496512, 257.3073905683720568, 14.20200298773971426 ) ) ;
#356 = CARTESIAN_POINT ( 'NONE',  ( -8.685887942688868435, 466.6823905765656377, 3.978247347593479866 ) ) ;
#357 = CARTESIAN_POINT ( 'NONE',  ( -45.43829269268871229, 415.0573905683721136, -3.332260488124726194 ) ) ;
#358 = DIRECTION ( 'NONE',  ( -1.000000000000000000, 0.000000000000000000, 0.000000000000000000 ) ) ;
#359 = CARTESIAN_POINT ( 'NONE',  ( 0.000000000000000000, 56.85652257517428865, 0.000000000000000000 ) ) ;
#360 = CARTESIAN_POINT ( 'NONE',  ( -48.68588794268887199, 272.3073905765655809, 3.978247347592742678 ) ) ;
#361 = CARTESIAN_POINT ( 'NONE',  ( -14.54375231895777176, 410.9948905601785327, 14.14213562373094568 ) ) ;
#362 = CARTESIAN_POINT ( 'NONE',  ( -22.27502019258948351, 332.2448905683720568, -15.47720386886985544 ) ) ;
#363 = CARTESIAN_POINT ( 'NONE',  ( -32.01814843081346140, 466.0573905683720000, 16.75240474999999307 ) ) ;
#364 = VERTEX_POINT ( 'NONE', #2756 ) ;
#365 = CARTESIAN_POINT ( 'NONE',  ( -8.685887942688736985, 471.9323905601784759, 3.978247347593161010 ) ) ;
#366 = CARTESIAN_POINT ( 'NONE',  ( -19.19641293061497578, 297.3073905683720568, 14.20200298773971426 ) ) ;
#367 = CARTESIAN_POINT ( 'NONE',  ( 0.000000000000000000, -5.629165124598843661, 3.250000000000012879 ) ) ;
#368 = VERTEX_POINT ( 'NONE', #4369 ) ;
#369 = CARTESIAN_POINT ( 'NONE',  ( -10.20829729246298356, 341.6198905601784759, 7.653668647301790529 ) ) ;
#370 = CARTESIAN_POINT ( 'NONE',  ( -25.35362745456399480, 392.5573905683720000, -16.75240474999999307 ) ) ;
#371 = CARTESIAN_POINT ( 'NONE',  ( -11.73070664223725679, 446.0573905765656377, 11.32908994701042005 ) ) ;
#372 = CARTESIAN_POINT ( 'NONE',  ( -42.88789093042844058, 432.9323905683720000, -9.489475012073736337 ) ) ;
#373 = CARTESIAN_POINT ( 'NONE',  ( -16.84014894278197616, 251.6198905683720284, -11.84573899990672707 ) ) ;
#374 = CARTESIAN_POINT ( 'NONE',  ( -35.09675569278795138, 421.9948905683720000, -15.47720386886985544 ) ) ;
#375 = SHAPE_DEFINITION_REPRESENTATION ( #12875, #7793 ) ;
#376 = VECTOR ( 'NONE', #7717, 1000.000000000000000 ) ;
#377 = DIRECTION ( 'NONE',  ( 1.000000000000000000, 0.000000000000000000, 0.000000000000000000 ) ) ;
#378 = CARTESIAN_POINT ( 'NONE',  ( -48.68588794268870856, 361.9948905765655809, 0.000000000000000000 ) ) ;
#379 = CARTESIAN_POINT ( 'NONE',  ( 6.416697501590670427, 172.9933428177121471, 45.00000000000000000 ) ) ;
#380 = CARTESIAN_POINT ( 'NONE',  ( -8.685887942688742314, 573.2448905601785327, 2.449293598294706119E-15 ) ) ;
#381 = CARTESIAN_POINT ( 'NONE',  ( -44.16309181155856578, 334.4948905683720568, 6.410867750099241924 ) ) ;
#382 = DIRECTION ( 'NONE',  ( -1.191790137725560488E-16, 1.000000000000000000, -0.000000000000000000 ) ) ;
#383 = CARTESIAN_POINT ( 'NONE',  ( -38.17536295476246266, 486.9323905683721136, 14.20200298773971781 ) ) ;
#384 = ADVANCED_FACE ( 'NONE', ( #21025 ), #9547, .F. ) ;
#385 = CARTESIAN_POINT ( 'NONE',  ( 30.42502041961813575, 271.1055109169419097, 20.00000000000000355 ) ) ;
#386 =( NAMED_UNIT ( * ) PLANE_ANGLE_UNIT ( ) SI_UNIT ( $, .RADIAN. ) );
#387 = CARTESIAN_POINT ( 'NONE',  ( 81.24038404635966515, 10.52886280891152104, -94.99999999999994316 ) ) ;
#388 = EDGE_CURVE ( 'NONE', #12297, #573, #12170, .T. ) ;
#389 = ADVANCED_FACE ( 'NONE', ( #7915 ), #13016, .F. ) ;
#390 =( GEOMETRIC_REPRESENTATION_CONTEXT ( 3 ) GLOBAL_UNCERTAINTY_ASSIGNED_CONTEXT ( ( #21302 ) ) GLOBAL_UNIT_ASSIGNED_CONTEXT ( ( #15423, #17981, #14445 ) ) REPRESENTATION_CONTEXT ( 'NONE', 'WORKASPACE' ) );
#391 = CARTESIAN_POINT ( 'NONE',  ( -45.43829269268871229, 385.3698905683720568, 0.000000000000000000 ) ) ;
#392 = CIRCLE ( 'NONE', #11415, 9.999999999999994671 ) ;
#393 = CARTESIAN_POINT ( 'NONE',  ( 81.24038404635966515, 10.52886280891152104, 94.99999999999994316 ) ) ;
#394 = CARTESIAN_POINT ( 'NONE',  ( -8.685887942688742314, 532.2448905601784190, -2.449293598294705724E-15 ) ) ;
#395 = CARTESIAN_POINT ( 'NONE',  ( -11.93348319268872260, 368.8698905683720000, -2.051577885510841163E-15 ) ) ;
#396 = ORIENTED_EDGE ( 'NONE', *, *, #3873, .T. ) ;
#397 = CARTESIAN_POINT ( 'NONE',  ( -38.17536295476246977, 525.4323905683720568, 14.20200298773971781 ) ) ;
#398 = ORIENTED_EDGE ( 'NONE', *, *, #15446, .F. ) ;
#399 = VECTOR ( 'NONE', #1589, 1000.000000000000000 ) ;
#400 = CARTESIAN_POINT ( 'NONE',  ( -25.35362745456400191, 526.6823905683720568, 16.75240474999998952 ) ) ;
#401 = EDGE_CURVE ( 'NONE', #17928, #21047, #11338, .T. ) ;
#402 = EDGE_LOOP ( 'NONE', ( #20811, #2569, #4602, #6698 ) ) ;
#403 = CARTESIAN_POINT ( 'NONE',  ( -40.01497788969913927, 428.8073905601784759, 16.95518130045146776 ) ) ;
#404 = CARTESIAN_POINT ( 'NONE',  ( -16.84014894278200103, 487.6198905683720000, 11.84573899990672530 ) ) ;
#405 = ORIENTED_EDGE ( 'NONE', *, *, #4592, .T. ) ;
#406 = CARTESIAN_POINT ( 'NONE',  ( -42.88789093042844769, 492.9323905683719431, -9.489475012073734561 ) ) ;
#407 = CARTESIAN_POINT ( 'NONE',  ( -28.68588794268872988, 47.23886018424757083, -49.60091809715359545 ) ) ;
#408 = VECTOR ( 'NONE', #5128, 1000.000000000000000 ) ;
#409 = CARTESIAN_POINT ( 'NONE',  ( -21.03221929538693047, 418.8698905765655809, -18.47759065022572855 ) ) ;
#410 = CARTESIAN_POINT ( 'NONE',  ( -11.73070664223726034, 476.0573905765656377, 11.32908994701042005 ) ) ;
#411 = DIRECTION ( 'NONE',  ( 0.000000000000000000, -1.000000000000000000, 0.000000000000000000 ) ) ;
#412 = DIRECTION ( 'NONE',  ( -1.000000000000000000, 0.000000000000000000, -0.000000000000000000 ) ) ;
#413 = DIRECTION ( 'NONE',  ( 0.000000000000000000, 0.000000000000000000, 1.000000000000000000 ) ) ;
#414 = FILL_AREA_STYLE_COLOUR ( '', #7996 ) ;
#415 = DIRECTION ( 'NONE',  ( 1.000000000000000000, 0.000000000000000000, 0.000000000000000000 ) ) ;
#416 = VECTOR ( 'NONE', #5059, 1000.000000000000000 ) ;
#417 = CARTESIAN_POINT ( 'NONE',  ( -32.01814843081344009, 293.1823905683720568, -16.75240474999999307 ) ) ;
#418 = PLANE ( 'NONE',  #13705 ) ;
#419 = CARTESIAN_POINT ( 'NONE',  ( -25.35362745456400191, 452.5573905683720568, -16.75240474999999307 ) ) ;
#420 = CARTESIAN_POINT ( 'NONE',  ( -40.01497788969913927, 413.5573905765656377, 16.95518130045146776 ) ) ;
#421 = CARTESIAN_POINT ( 'NONE',  ( -25.35362745456398059, 272.5573905683721136, -16.75240474999999307 ) ) ;
#422 = ORIENTED_EDGE ( 'NONE', *, *, #2699, .T. ) ;
#423 = DIRECTION ( 'NONE',  ( 1.000000000000000000, 0.000000000000000000, -0.000000000000000000 ) ) ;
#424 = VECTOR ( 'NONE', #12547, 1000.000000000000000 ) ;
#425 = CARTESIAN_POINT ( 'NONE',  ( -38.17536295476246266, 496.9323905683720568, 14.20200298773971781 ) ) ;
#426 = ORIENTED_EDGE ( 'NONE', *, *, #17683, .T. ) ;
#427 = CARTESIAN_POINT ( 'NONE',  ( -22.27502019258948707, 458.4948905683720568, 15.47720386886985189 ) ) ;
#428 = CARTESIAN_POINT ( 'NONE',  ( 30.07572094023280940, 170.1716627696692683, -57.31989048965873934 ) ) ;
#429 = CARTESIAN_POINT ( 'NONE',  ( -13.20868407381884779, 258.2448905683720000, 6.410867750099229490 ) ) ;
#430 = ORIENTED_EDGE ( 'NONE', *, *, #1923, .F. ) ;
#431 = FACE_OUTER_BOUND ( 'NONE', #16031, .T. ) ;
#432 = CARTESIAN_POINT ( 'NONE',  ( -13.20868407381884779, 250.9948905683720284, -6.410867750099233042 ) ) ;
#433 = CARTESIAN_POINT ( 'NONE',  ( 5.299999999999999822, 5.388445916248354013E-16, 4.400000000000000355 ) ) ;
#434 = DIRECTION ( 'NONE',  ( -1.191790137725560488E-16, 1.000000000000000000, -0.000000000000000000 ) ) ;
#435 = CARTESIAN_POINT ( 'NONE',  ( -11.93348319268871016, 259.1823905683720000, -3.332260488124732856 ) ) ;
#436 = CARTESIAN_POINT ( 'NONE',  ( -22.27502019258948707, 362.2448905683720000, -15.47720386886985544 ) ) ;
#437 = ADVANCED_FACE ( 'NONE', ( #268 ), #19715, .T. ) ;
#438 = DIRECTION ( 'NONE',  ( 0.000000000000000000, -1.000000000000000000, 0.000000000000000000 ) ) ;
#439 = CARTESIAN_POINT ( 'NONE',  ( -25.35362745456398770, 406.6823905683720000, 16.75240474999998952 ) ) ;
#440 = EDGE_CURVE ( 'NONE', #16030, #15607, #16966, .T. ) ;
#441 = CARTESIAN_POINT ( 'NONE',  ( -36.33955658999053639, 509.1198905601784759, 18.47759065022572500 ) ) ;
#442 = CARTESIAN_POINT ( 'NONE',  ( -45.64106924314019409, 416.3073905601784759, -11.32908994701042715 ) ) ;
#443 = ORIENTED_EDGE ( 'NONE', *, *, #8517, .T. ) ;
#444 = DIRECTION ( 'NONE',  ( 0.000000000000000000, 1.000000000000000000, -0.000000000000000000 ) ) ;
#445 = VERTEX_POINT ( 'NONE', #10184 ) ;
#446 = ORIENTED_EDGE ( 'NONE', *, *, #9956, .F. ) ;
#447 = CARTESIAN_POINT ( 'NONE',  ( -32.01814843081346851, 527.5573905683720568, 16.75240474999999307 ) ) ;
#448 = CARTESIAN_POINT ( 'NONE',  ( -42.82802356641965247, 295.9948905601784759, -14.14213562373094746 ) ) ;
#449 = CARTESIAN_POINT ( 'NONE',  ( -47.16347859291443712, 321.3698905765656377, -7.653668647301793193 ) ) ;
#450 = AXIS2_PLACEMENT_3D ( 'NONE', #15921, #17640, #8987 ) ;
#451 = VERTEX_POINT ( 'NONE', #3287 ) ;
#452 = CARTESIAN_POINT ( 'NONE',  ( -44.16309181155855867, 315.9948905683720568, 6.410867750099241924 ) ) ;
#453 = EDGE_CURVE ( 'NONE', #17091, #12371, #14396, .T. ) ;
#454 = VERTEX_POINT ( 'NONE', #16805 ) ;
#455 = CARTESIAN_POINT ( 'NONE',  ( -11.93348319268872260, 339.1823905683720568, -3.332260488124732856 ) ) ;
#456 = CARTESIAN_POINT ( 'NONE',  ( -25.35362745456399125, 371.0573905683719431, -16.75240474999999307 ) ) ;
#457 = CARTESIAN_POINT ( 'NONE',  ( -36.33955658999050797, 293.8698905765656377, 18.47759065022572500 ) ) ;
#458 = DIRECTION ( 'NONE',  ( 0.000000000000000000, 0.000000000000000000, -1.000000000000000000 ) ) ;
#459 = CARTESIAN_POINT ( 'NONE',  ( -40.53162694259543031, 272.6198905683720568, -11.84573899990672707 ) ) ;
#460 = CARTESIAN_POINT ( 'NONE',  ( -28.68588794268872633, 464.4948905765656377, 19.99999999999999289 ) ) ;
#461 = VECTOR ( 'NONE', #11102, 1000.000000000000000 ) ;
#462 = CARTESIAN_POINT ( 'NONE',  ( -22.27502019258948351, 418.4948905683720000, 15.47720386886985189 ) ) ;
#463 = ADVANCED_FACE ( 'NONE', ( #4898 ), #18196, .F. ) ;
#464 = CARTESIAN_POINT ( 'NONE',  ( -26.01014438536011397, 45.91972051657856468, 122.2644972899424687 ) ) ;
#465 = CARTESIAN_POINT ( 'NONE',  ( -10.20829729246299600, 447.6198905765656377, -7.653668647301794969 ) ) ;
#466 = LINE ( 'NONE', #566, #15334 ) ;
#467 = CARTESIAN_POINT ( 'NONE',  ( -16.84014894278198327, 329.1198905683720568, 11.84573899990672530 ) ) ;
#468 = CARTESIAN_POINT ( 'NONE',  ( -14.48388495494900852, 467.9323905683721136, 9.489475012073732785 ) ) ;
#469 = VERTEX_POINT ( 'NONE', #13128 ) ;
#470 = CARTESIAN_POINT ( 'NONE',  ( -36.33955658999052218, 465.3698905601784759, -18.47759065022572855 ) ) ;
#471 = CARTESIAN_POINT ( 'NONE',  ( -13.20868407381885135, 289.4948905683720000, -6.410867750099233042 ) ) ;
#472 = AXIS2_PLACEMENT_3D ( 'NONE', #710, #4366, #2536 ) ;
#473 = ORIENTED_EDGE ( 'NONE', *, *, #19536, .T. ) ;
#474 = CARTESIAN_POINT ( 'NONE',  ( -28.68588794268871212, 344.4948905765656377, 19.99999999999999289 ) ) ;
#475 = ORIENTED_EDGE ( 'NONE', *, *, #15442, .F. ) ;
#476 = CARTESIAN_POINT ( 'NONE',  ( -33.07955326574333554, 585.7448905601785327, -10.74819839862556314 ) ) ;
#477 = CARTESIAN_POINT ( 'NONE',  ( -47.16347859291444422, 346.6198905601784190, -7.653668647301793193 ) ) ;
#478 =( REPRESENTATION_RELATIONSHIP ('NONE','NONE', #1888, #8616 ) REPRESENTATION_RELATIONSHIP_WITH_TRANSFORMATION ( #20684 )SHAPE_REPRESENTATION_RELATIONSHIP( ) );
#479 = AXIS2_PLACEMENT_3D ( 'NONE', #7986, #1737, #16125 ) ;
#480 = CARTESIAN_POINT ( 'NONE',  ( -25.35362745456398414, 301.0573905683720568, -16.75240474999999307 ) ) ;
#481 = EDGE_CURVE ( 'NONE', #18883, #10793, #10717, .T. ) ;
#482 = CARTESIAN_POINT ( 'NONE',  ( -19.19641293061498644, 391.9323905683720568, -14.20200298773971603 ) ) ;
#483 = DIRECTION ( 'NONE',  ( 0.000000000000000000, -1.000000000000000000, 0.000000000000000000 ) ) ;
#484 = CARTESIAN_POINT ( 'NONE',  ( -38.17536295476245556, 425.4323905683720000, 14.20200298773971781 ) ) ;
#485 = CARTESIAN_POINT ( 'NONE',  ( -40.53162694259542320, 256.6198905683720568, 11.84573899990672885 ) ) ;
#486 = CARTESIAN_POINT ( 'NONE',  ( -16.84014894278199392, 417.6198905683720000, 11.84573899990672530 ) ) ;
#487 = APPLICATION_PROTOCOL_DEFINITION ( 'draft international standard', 'automotive_design', 1998, #14845 ) ;
#488 = CARTESIAN_POINT ( 'NONE',  ( -48.68588794268870856, 362.3073905765656377, 3.978247347593168115 ) ) ;
#489 = LINE ( 'NONE', #7156, #6873 ) ;
#490 = CARTESIAN_POINT ( 'NONE',  ( -19.19641293061497933, 320.4323905683720000, -14.20200298773971603 ) ) ;
#491 = CARTESIAN_POINT ( 'NONE',  ( -14.48388495494901385, 481.3073905683720000, -9.489475012073736337 ) ) ;
#492 = EDGE_CURVE ( 'NONE', #4291, #6162, #10377, .T. ) ;
#493 = AXIS2_PLACEMENT_3D ( 'NONE', #1831, #8402, #15027 ) ;
#494 = CARTESIAN_POINT ( 'NONE',  ( 81.24038404635965094, 10.52886280891152104, -131.1729372809869005 ) ) ;
#495 = DIRECTION ( 'NONE',  ( 0.000000000000000000, 0.000000000000000000, 1.000000000000000000 ) ) ;
#496 = AXIS2_PLACEMENT_3D ( 'NONE', #18707, #14078, #15484 ) ;
#497 = CARTESIAN_POINT ( 'NONE',  ( -44.16309181155857289, 395.9948905683720568, 6.410867750099241924 ) ) ;
#498 = DIRECTION ( 'NONE',  ( 0.000000000000000000, 1.000000000000000000, 0.000000000000000000 ) ) ;
#499 =( BOUNDED_CURVE ( )  B_SPLINE_CURVE ( 2, ( #11343, #1515, #13084, #19671, #3244, #5381, #19892, #3874, #13412, #10462, #3766, #13307, #2053, #18372, #16664, #5070, #11672 ),
 .UNSPECIFIED., .F., .T. ) 
 B_SPLINE_CURVE_WITH_KNOTS ( ( 3, 2, 2, 2, 2, 2, 2, 2, 3 ),
 ( 0.7968750000000002220, 0.7988281250000002220, 0.8007812500000002220, 0.8027343750000002220, 0.8046875000000002220, 0.8066406250000002220, 0.8085937500000002220, 0.8105468750000002220, 0.8125000000000002220 ),
 .UNSPECIFIED. ) 
 CURVE ( )  GEOMETRIC_REPRESENTATION_ITEM ( )  RATIONAL_B_SPLINE_CURVE ( ( 0.9999999999999977796, 0.9807852804032326510, 1.000000000000000000, 0.9807852804032304306, 1.000000000000000000, 0.9807852804032304306, 1.000000000000000000, 0.9807852804032304306, 1.000000000000000000, 0.9807852804032304306, 1.000000000000000000, 0.9807852804032304306, 1.000000000000000000, 0.9807852804032304306, 1.000000000000000000, 0.9807852804032282101, 1.000000000000002220 ) ) 
 REPRESENTATION_ITEM ( '' )  );
#500 = CARTESIAN_POINT ( 'NONE',  ( -17.35679799567831694, 533.8073905601784190, -16.95518130045146421 ) ) ;
#501 = CARTESIAN_POINT ( 'NONE',  ( -28.68588794268871212, 346.3698905683720568, 16.75240474999999307 ) ) ;
#502 = VERTEX_POINT ( 'NONE', #1782 ) ;
#503 = CARTESIAN_POINT ( 'NONE',  ( -35.09675569278797269, 525.7448905683720568, 15.47720386886985366 ) ) ;
#504 = EDGE_LOOP ( 'NONE', ( #18852, #5687, #1345, #9828 ) ) ;
#505 = CARTESIAN_POINT ( 'NONE',  ( -44.16309181155859420, 513.2448905683719431, -6.410867750099231266 ) ) ;
#506 = ORIENTED_EDGE ( 'NONE', *, *, #5396, .F. ) ;
#507 = CARTESIAN_POINT ( 'NONE',  ( -45.64106924314018698, 428.1823905601784190, 11.32908994701042538 ) ) ;
#508 = CARTESIAN_POINT ( 'NONE',  ( -40.53162694259545162, 475.1198905683720000, 11.84573899990672885 ) ) ;
#509 = ORIENTED_EDGE ( 'NONE', *, *, #7343, .F. ) ;
#510 = CARTESIAN_POINT ( 'NONE',  ( -45.43829269268872650, 494.1823905683720000, 3.332260488124734632 ) ) ;
#511 = CARTESIAN_POINT ( 'NONE',  ( -14.54375231895778242, 490.9948905601784759, 14.14213562373094568 ) ) ;
#512 = AXIS2_PLACEMENT_3D ( 'NONE', #229, #20006, #5182 ) ;
#513 = CARTESIAN_POINT ( 'NONE',  ( -32.66413529028188378, 424.1823905765656377, 19.99999999999999289 ) ) ;
#514 = CARTESIAN_POINT ( 'NONE',  ( 52.60622592008805043, 30.52886280891152282, -151.0302712373927250 ) ) ;
#515 = CARTESIAN_POINT ( 'NONE',  ( -28.68588794268870501, 299.7448905601784759, 19.99999999999999289 ) ) ;
#516 = CARTESIAN_POINT ( 'NONE',  ( -14.54375231895778064, 438.2448905765656377, -14.14213562373094746 ) ) ;
#517 = CARTESIAN_POINT ( 'NONE',  ( -64.27068722059112815, 600.7448905601785327, -35.12437985717895828 ) ) ;
#518 = DIRECTION ( 'NONE',  ( 1.191790137725560488E-16, -1.000000000000000000, -0.000000000000000000 ) ) ;
#519 = DIRECTION ( 'NONE',  ( -1.191790137725560488E-16, 1.000000000000000000, 0.000000000000000000 ) ) ;
#520 = EDGE_CURVE ( 'NONE', #232, #14361, #20193, .T. ) ;
#521 = CARTESIAN_POINT ( 'NONE',  ( -42.88789093042842637, 294.4323905683720568, -9.489475012073736337 ) ) ;
#522 = EDGE_CURVE ( 'NONE', #2119, #5209, #10396, .T. ) ;
#523 = CARTESIAN_POINT ( 'NONE',  ( -48.68588794268871567, 437.2448905601785327, 0.000000000000000000 ) ) ;
#524 = CARTESIAN_POINT ( 'NONE',  ( -38.17536295476246977, 453.8073905683720568, -14.20200298773971426 ) ) ;
#525 = DIRECTION ( 'NONE',  ( -0.000000000000000000, -0.000000000000000000, -1.000000000000000000 ) ) ;
#526 = CARTESIAN_POINT ( 'NONE',  ( -11.93348319268871194, 270.6823905683719431, -3.332260488124732856 ) ) ;
#527 = ORIENTED_EDGE ( 'NONE', *, *, #5440, .F. ) ;
#528 = CARTESIAN_POINT ( 'NONE',  ( -48.68588794268886488, 267.5573905601783622, 3.978247347592742678 ) ) ;
#529 = CARTESIAN_POINT ( 'NONE',  ( -32.01814843081345430, 487.5573905683720568, 16.75240474999999307 ) ) ;
#530 = ORIENTED_EDGE ( 'NONE', *, *, #2479, .F. ) ;
#531 = CARTESIAN_POINT ( 'NONE',  ( -22.27502019258949773, 462.2448905683720568, -15.47720386886985544 ) ) ;
#532 = CARTESIAN_POINT ( 'NONE',  ( -28.68588794268874054, 573.2448905601785327, 0.000000000000000000 ) ) ;
#533 = CARTESIAN_POINT ( 'NONE',  ( -40.53162694259542320, 252.6198905683720284, -11.84573899990672707 ) ) ;
#534 = VERTEX_POINT ( 'NONE', #5742 ) ;
#535 = DIRECTION ( 'NONE',  ( -1.000000000000000000, 0.000000000000000000, 0.000000000000000000 ) ) ;
#536 = CARTESIAN_POINT ( 'NONE',  ( -17.35679799567830628, 485.4323905765656946, 16.95518130045146421 ) ) ;
#537 = CARTESIAN_POINT ( 'NONE',  ( -24.70764059509555111, 390.0573905601784759, 19.99999999999998934 ) ) ;
#538 = CARTESIAN_POINT ( 'NONE',  ( -11.93348319268870661, 250.0573905683720000, 3.332260488124728859 ) ) ;
#539 = CARTESIAN_POINT ( 'NONE',  ( -42.82802356641966668, 420.7448905765656377, -14.14213562373094746 ) ) ;
#540 = CARTESIAN_POINT ( 'NONE',  ( -1.592577856902392952, 222.3338630624045607, -7.432224998792205994 ) ) ;
#541 = CARTESIAN_POINT ( 'NONE',  ( -14.48388495494898365, 237.9323905683720000, 9.489475012073732785 ) ) ;
#542 = CARTESIAN_POINT ( 'NONE',  ( -35.09675569278794427, 353.4948905683720000, -15.47720386886985544 ) ) ;
#543 = CARTESIAN_POINT ( 'NONE',  ( 10.41669750159067220, 217.7548513357008630, 45.00000000000000000 ) ) ;
#544 = CARTESIAN_POINT ( 'NONE',  ( -13.20868407381886378, 398.2448905683720568, 6.410867750099229490 ) ) ;
#545 = CARTESIAN_POINT ( 'NONE',  ( -11.73070664223725501, 413.1823905601784190, -11.32908994701042715 ) ) ;
#546 = ORIENTED_EDGE ( 'NONE', *, *, #13520, .F. ) ;
#547 = PLANE ( 'NONE',  #5292 ) ;
#548 = EDGE_LOOP ( 'NONE', ( #5390, #12592, #4680 ) ) ;
#549 = ORIENTED_EDGE ( 'NONE', *, *, #4990, .T. ) ;
#550 = CARTESIAN_POINT ( 'NONE',  ( -38.17536295476247687, 523.8073905683720568, -14.20200298773971426 ) ) ;
#551 = CARTESIAN_POINT ( 'NONE',  ( -28.68588794268870146, 279.7448905601784759, 19.99999999999999289 ) ) ;
#552 = CARTESIAN_POINT ( 'NONE',  ( -28.68588794268871212, 319.4948905765656377, -19.99999999999999289 ) ) ;
#553 = CARTESIAN_POINT ( 'NONE',  ( -11.93348319268871549, 320.3698905683720568, -2.051577885510841163E-15 ) ) ;
#554 = VERTEX_POINT ( 'NONE', #14098 ) ;
#555 = CARTESIAN_POINT ( 'NONE',  ( -40.53162694259543741, 352.6198905683720000, -11.84573899990672707 ) ) ;
#556 = CARTESIAN_POINT ( 'NONE',  ( -22.27502019258947641, 356.9948905683720000, 15.47720386886985189 ) ) ;
#557 = EDGE_CURVE ( 'NONE', #10903, #18972, #18791, .T. ) ;
#558 = CARTESIAN_POINT ( 'NONE',  ( -36.33955658999050797, 273.8698905765656377, 18.47759065022572500 ) ) ;
#559 = CARTESIAN_POINT ( 'NONE',  ( -48.68588794268873698, 573.2448905601785327, 0.000000000000000000 ) ) ;
#560 = EDGE_CURVE ( 'NONE', #9549, #9782, #17331, .T. ) ;
#561 = CARTESIAN_POINT ( 'NONE',  ( -40.53162694259542320, 262.6198905683720568, -11.84573899990672707 ) ) ;
#562 = CARTESIAN_POINT ( 'NONE',  ( -43.20748696942036560, 201.8382954020867999, 3.765466433758052123 ) ) ;
#563 = CARTESIAN_POINT ( 'NONE',  ( -13.20868407381886378, 409.7448905683720000, 6.410867750099229490 ) ) ;
#564 = CARTESIAN_POINT ( 'NONE',  ( -48.68588794268854514, 336.9323905601784190, -3.978247347593583783 ) ) ;
#565 = CARTESIAN_POINT ( 'NONE',  ( -36.33955658999050797, 355.3698905601784759, -18.47759065022572855 ) ) ;
#566 = CARTESIAN_POINT ( 'NONE',  ( -74.06037022053952512, 10.52886280891152104, -40.00000000000000000 ) ) ;
#567 = CARTESIAN_POINT ( 'NONE',  ( -44.16309181155856578, 324.7448905683720000, -6.410867750099231266 ) ) ;
#568 = CARTESIAN_POINT ( 'NONE',  ( -11.93348319268873325, 459.1823905683720000, -3.332260488124732856 ) ) ;
#569 = ORIENTED_EDGE ( 'NONE', *, *, #6635, .T. ) ;
#570 = CARTESIAN_POINT ( 'NONE',  ( -45.64106924314020119, 468.1823905601785327, 11.32908994701042715 ) ) ;
#571 = CARTESIAN_POINT ( 'NONE',  ( -22.27502019258947996, 290.7448905683720568, -15.47720386886985544 ) ) ;
#572 = EDGE_LOOP ( 'NONE', ( #20946, #19765, #20650 ) ) ;
#573 = VERTEX_POINT ( 'NONE', #9099 ) ;
#574 = LINE ( 'NONE', #265, #16749 ) ;
#575 = CARTESIAN_POINT ( 'NONE',  ( -45.64106924314018698, 346.3073905601784759, -11.32908994701042715 ) ) ;
#576 = CARTESIAN_POINT ( 'NONE',  ( -19.19641293061497933, 310.4323905683720568, -14.20200298773971603 ) ) ;
#577 = EDGE_CURVE ( 'NONE', #15582, #9825, #9690, .T. ) ;
#578 = CARTESIAN_POINT ( 'NONE',  ( -45.43829269268871229, 375.6823905683720000, 3.332260488124734632 ) ) ;
#579 = CONICAL_SURFACE ( 'NONE', #20253, 3.309499999999999886, 0.7853981633974432830 ) ;
#580 = CARTESIAN_POINT ( 'NONE',  ( -24.70764059509552979, 230.0573905601784759, 19.99999999999998934 ) ) ;
#581 = B_SPLINE_CURVE_WITH_KNOTS ( 'NONE', 3,
 ( #18974, #14022, #18860, #15748, #7605, #8810 ),
 .UNSPECIFIED., .F., .F.,
 ( 4, 2, 4 ),
 ( 2.380733003139562229E-07, 0.001898835937927375716, 0.003797433802554437202 ),
 .UNSPECIFIED. ) ;
#582 = CARTESIAN_POINT ( 'NONE',  ( -10.20829729246300666, 527.6198905765656946, -7.653668647301794969 ) ) ;
#583 = CARTESIAN_POINT ( 'NONE',  ( -22.27502019258949062, 400.7448905683720568, -15.47720386886985544 ) ) ;
#584 = CARTESIAN_POINT ( 'NONE',  ( -44.16309181155855867, 254.7448905683720284, -6.410867750099231266 ) ) ;
#585 = CARTESIAN_POINT ( 'NONE',  ( -38.17536295476246266, 432.3073905683720000, -14.20200298773971426 ) ) ;
#586 = VECTOR ( 'NONE', #7728, 1000.000000000000114 ) ;
#587 = CARTESIAN_POINT ( 'NONE',  ( -45.64106924314018698, 342.9323905765655809, 11.32908994701042715 ) ) ;
#588 = CARTESIAN_POINT ( 'NONE',  ( 35.96497763894178945, 230.5765313837437418, -40.00000000000000000 ) ) ;
#589 = CARTESIAN_POINT ( 'NONE',  ( -11.93348319268871727, 328.8698905683720000, -2.051577885510841163E-15 ) ) ;
#590 =( NAMED_UNIT ( * ) SI_UNIT ( $, .STERADIAN. ) SOLID_ANGLE_UNIT ( ) );
#591 = CARTESIAN_POINT ( 'NONE',  ( -44.16309181155857999, 485.9948905683720568, 6.410867750099241924 ) ) ;
#592 = DIRECTION ( 'NONE',  ( -0.000000000000000000, -0.000000000000000000, -1.000000000000000000 ) ) ;
#593 = CARTESIAN_POINT ( 'NONE',  ( -42.91927816222971614, 203.5270276421415190, -4.734255112268845878 ) ) ;
#594 = CARTESIAN_POINT ( 'NONE',  ( -28.68588794268869435, 224.4948905765656377, 19.99999999999999289 ) ) ;
#595 = EDGE_CURVE ( 'NONE', #1881, #15561, #10610, .T. ) ;
#596 = CIRCLE ( 'NONE', #11637, 4.000000000000003553 ) ;
#597 = CARTESIAN_POINT ( 'NONE',  ( -32.01814843081344719, 387.5573905683719431, 16.75240474999999307 ) ) ;
#598 = LINE ( 'NONE', #13897, #14420 ) ;
#599 = CARTESIAN_POINT ( 'NONE',  ( -40.01497788969915348, 518.8073905601785327, 16.95518130045146776 ) ) ;
#600 = CARTESIAN_POINT ( 'NONE',  ( -11.93348319268872260, 339.1823905683720568, -3.332260488124732856 ) ) ;
#601 = VECTOR ( 'NONE', #13140, 999.9999999999998863 ) ;
#602 = ORIENTED_EDGE ( 'NONE', *, *, #17756, .T. ) ;
#603 = CARTESIAN_POINT ( 'NONE',  ( -11.93348319268873858, 508.5573905683720000, 3.332260488124728415 ) ) ;
#604 = VERTEX_POINT ( 'NONE', #20679 ) ;
#605 = CARTESIAN_POINT ( 'NONE',  ( -43.23114467231988556, 223.9102039777116033, -8.415129624329841462 ) ) ;
#606 = LINE ( 'NONE', #100, #18425 ) ;
#607 = EDGE_CURVE ( 'NONE', #10104, #12829, #18832, .T. ) ;
#608 = CARTESIAN_POINT ( 'NONE',  ( -28.68588794268874054, 271.1055109169419666, 40.00000000000000000 ) ) ;
#609 = CARTESIAN_POINT ( 'NONE',  ( -45.43829269268871940, 473.5573905683720000, -3.332260488124726194 ) ) ;
#610 = ORIENTED_EDGE ( 'NONE', *, *, #4427, .T. ) ;
#611 = CARTESIAN_POINT ( 'NONE',  ( -28.68588794268872633, 486.3698905683720568, 16.75240474999999307 ) ) ;
#612 = CARTESIAN_POINT ( 'NONE',  ( -24.70764059509553334, 244.8073905765656377, 19.99999999999998934 ) ) ;
#613 = VECTOR ( 'NONE', #276, 1000.000000000000000 ) ;
#614 = CARTESIAN_POINT ( 'NONE',  ( -21.03221929538691626, 415.1198905765656377, 18.47759065022572500 ) ) ;
#615 = LINE ( 'NONE', #17154, #5483 ) ;
#616 = DIRECTION ( 'NONE',  ( -1.191790137725560488E-16, 1.000000000000000000, -0.000000000000000000 ) ) ;
#617 = CARTESIAN_POINT ( 'NONE',  ( 6.416697501590670427, 172.9933428177121471, 49.99999999999999289 ) ) ;
#618 = PLANE ( 'NONE',  #17372 ) ;
#619 = CONICAL_SURFACE ( 'NONE', #12351, 3.309499999999999886, 0.7853981633974407295 ) ;
#620 = CARTESIAN_POINT ( 'NONE',  ( -32.66413529028185536, 259.8073905765655809, -19.99999999999999289 ) ) ;
#621 =( NAMED_UNIT ( * ) SI_UNIT ( $, .STERADIAN. ) SOLID_ANGLE_UNIT ( ) );
#622 = CARTESIAN_POINT ( 'NONE',  ( -28.68588794268874764, 575.7448905601785327, 0.000000000000000000 ) ) ;
#623 =( BOUNDED_CURVE ( )  B_SPLINE_CURVE ( 2, ( #14337, #9648, #9329, #17771, #1236, #2749, #13124, #7910, #16269, #7808, #4893, #11168, #14440, #21020, #2962, #16160, #6190 ),
 .UNSPECIFIED., .F., .T. ) 
 B_SPLINE_CURVE_WITH_KNOTS ( ( 3, 2, 2, 2, 2, 2, 2, 2, 3 ),
 ( 0.03125000000000002776, 0.03320312500000007633, 0.03515625000000012490, 0.03710937500000016653, 0.03906250000000021511, 0.04101562500000026368, 0.04296875000000030531, 0.04492187500000035388, 0.04687500000000040246 ),
 .UNSPECIFIED. ) 
 CURVE ( )  GEOMETRIC_REPRESENTATION_ITEM ( )  RATIONAL_B_SPLINE_CURVE ( ( 0.9999999999999997780, 0.9807852804032306526, 1.000000000000000000, 0.9807852804032304306, 1.000000000000000000, 0.9807852804032304306, 1.000000000000000000, 0.9807852804032304306, 1.000000000000000000, 0.9807852804032304306, 1.000000000000000000, 0.9807852804032304306, 1.000000000000000000, 0.9807852804032304306, 1.000000000000000000, 0.9807852804032264338, 1.000000000000003997 ) ) 
 REPRESENTATION_ITEM ( '' )  );
#624 = CARTESIAN_POINT ( 'NONE',  ( -25.35362745456398059, 272.5573905683721136, -16.75240474999999307 ) ) ;
#625 = CARTESIAN_POINT ( 'NONE',  ( -24.70764059509555466, 404.8073905765656946, 19.99999999999998934 ) ) ;
#626 = CARTESIAN_POINT ( 'NONE',  ( -32.01814843081346140, 453.1823905683720568, -16.75240474999999307 ) ) ;
#627 = CARTESIAN_POINT ( 'NONE',  ( -45.64106924314018698, 401.0573905765655809, -11.32908994701042538 ) ) ;
#628 = CARTESIAN_POINT ( 'NONE',  ( -22.27502019258947641, 262.2448905683720000, -15.47720386886985544 ) ) ;
#629 = VERTEX_POINT ( 'NONE', #10503 ) ;
#630 = CARTESIAN_POINT ( 'NONE',  ( -10.20829729246297646, 271.6198905601784759, 7.653668647301790529 ) ) ;
#631 = CARTESIAN_POINT ( 'NONE',  ( -28.68588794268873343, 492.8698905683720568, -16.75240474999999307 ) ) ;
#632 = ORIENTED_EDGE ( 'NONE', *, *, #5260, .T. ) ;
#633 = CARTESIAN_POINT ( 'NONE',  ( 147.4234352242185935, 610.7448905601785327, 1.893624729818134345 ) ) ;
#634 = CARTESIAN_POINT ( 'NONE',  ( -13.20868407381884779, 268.2448905683720568, 6.410867750099229490 ) ) ;
#635 = EDGE_CURVE ( 'NONE', #15132, #11572, #2303, .T. ) ;
#636 = ORIENTED_EDGE ( 'NONE', *, *, #9399, .F. ) ;
#637 = LINE ( 'NONE', #11877, #10739 ) ;
#638 = CARTESIAN_POINT ( 'NONE',  ( -17.35679799567831338, 488.5573905765656377, -16.95518130045146421 ) ) ;
#639 = CARTESIAN_POINT ( 'NONE',  ( -28.68588794268873698, 10.52886280891152104, 0.000000000000000000 ) ) ;
#640 = CARTESIAN_POINT ( 'NONE',  ( -29.83144594096557967, 223.9102039777117170, -18.35382411513653267 ) ) ;
#641 = CARTESIAN_POINT ( 'NONE',  ( -19.19641293061496867, 241.9323905683720000, -14.20200298773971603 ) ) ;
#642 = CARTESIAN_POINT ( 'NONE',  ( -19.19641293061500420, 521.9323905683720568, -14.20200298773971603 ) ) ;
#643 = CARTESIAN_POINT ( 'NONE',  ( -17.35679799567829207, 375.4323905765655809, 16.95518130045146421 ) ) ;
#644 = CARTESIAN_POINT ( 'NONE',  ( -25.35362745456396638, 256.6823905683720000, 16.75240474999998952 ) ) ;
#645 = CARTESIAN_POINT ( 'NONE',  ( -25.35362745456398770, 342.5573905683720568, -16.75240474999999307 ) ) ;
#646 = EDGE_CURVE ( 'NONE', #8266, #13560, #21015, .T. ) ;
#647 = CARTESIAN_POINT ( 'NONE',  ( 60.03793209889851568, 30.52886280891152282, 131.1729372809869005 ) ) ;
#648 = EDGE_CURVE ( 'NONE', #8661, #6220, #4165, .T. ) ;
#649 = ADVANCED_FACE ( 'NONE', ( #4241 ), #12780, .T. ) ;
#650 = CARTESIAN_POINT ( 'NONE',  ( -38.17536295476245556, 405.4323905683721136, 14.20200298773971781 ) ) ;
#651 = DIRECTION ( 'NONE',  ( -0.000000000000000000, -0.000000000000000000, 1.000000000000000000 ) ) ;
#652 = CARTESIAN_POINT ( 'NONE',  ( -11.73070664223725146, 411.3073905601784759, 11.32908994701042005 ) ) ;
#653 = CIRCLE ( 'NONE', #14480, 21.20245194746113526 ) ;
#654 = ORIENTED_EDGE ( 'NONE', *, *, #11731, .T. ) ;
#655 = DIRECTION ( 'NONE',  ( 0.000000000000000000, -0.000000000000000000, 1.000000000000000000 ) ) ;
#656 = ORIENTED_EDGE ( 'NONE', *, *, #14084, .F. ) ;
#657 = ORIENTED_EDGE ( 'NONE', *, *, #20933, .F. ) ;
#658 = CARTESIAN_POINT ( 'NONE',  ( -35.09675569278795848, 503.4948905683720568, -15.47720386886985544 ) ) ;
#659 = CARTESIAN_POINT ( 'NONE',  ( -10.20829729246297646, 291.6198905601784759, 7.653668647301790529 ) ) ;
#660 = CARTESIAN_POINT ( 'NONE',  ( -43.68588794268869435, 210.1437886375728965, 2.161863591991830530E-19 ) ) ;
#661 = VERTEX_POINT ( 'NONE', #1116 ) ;
#662 = EDGE_CURVE ( 'NONE', #19239, #10847, #8186, .T. ) ;
#663 = CARTESIAN_POINT ( 'NONE',  ( -22.27502019258948351, 322.2448905683720000, -15.47720386886985544 ) ) ;
#664 = CARTESIAN_POINT ( 'NONE',  ( -44.16309181155857289, 343.2448905683720000, -6.410867750099231266 ) ) ;
#665 = CARTESIAN_POINT ( 'NONE',  ( -42.88789093042843348, 364.8073905683720568, 9.489475012073734561 ) ) ;
#666 = CARTESIAN_POINT ( 'NONE',  ( -48.68588794268870146, 292.3073905765656377, 3.978247347593168115 ) ) ;
#667 = CARTESIAN_POINT ( 'NONE',  ( -24.70764059509557597, 499.1823905765655809, -19.99999999999999289 ) ) ;
#668 = CARTESIAN_POINT ( 'NONE',  ( -11.93348319268870661, 248.8698905683720000, -2.051577885510841163E-15 ) ) ;
#669 = CARTESIAN_POINT ( 'NONE',  ( -28.68588794268872633, 333.8848358243226357, 0.000000000000000000 ) ) ;
#670 = CARTESIAN_POINT ( 'NONE',  ( -14.48388495494900496, 409.4323905683720000, 9.489475012073732785 ) ) ;
#671 = AXIS2_PLACEMENT_3D ( 'NONE', #5649, #6070, #7583 ) ;
#672 = CARTESIAN_POINT ( 'NONE',  ( -40.01497788969913927, 335.6823905601785327, -16.95518130045146421 ) ) ;
#673 = DIRECTION ( 'NONE',  ( 1.000000000000000000, 0.000000000000000000, -0.000000000000000000 ) ) ;
#674 = CARTESIAN_POINT ( 'NONE',  ( -1.025382690249029949, 326.0737056351150613, 25.00000000000000000 ) ) ;
#675 = CARTESIAN_POINT ( 'NONE',  ( -44.16309181155857289, 334.7448905683720568, -6.410867750099231266 ) ) ;
#676 = CARTESIAN_POINT ( 'NONE',  ( -38.17536295476246266, 455.4323905683720000, 14.20200298773971781 ) ) ;
#677 = ORIENTED_EDGE ( 'NONE', *, *, #8682, .F. ) ;
#678 = CARTESIAN_POINT ( 'NONE',  ( -28.68588794268872633, 469.7448905601784759, 19.99999999999999289 ) ) ;
#679 = CARTESIAN_POINT ( 'NONE',  ( -35.09675569278793716, 281.9948905683720000, -15.47720386886985544 ) ) ;
#680 = EDGE_LOOP ( 'NONE', ( #16620, #509, #5345, #8208 ) ) ;
#681 = CARTESIAN_POINT ( 'NONE',  ( -45.64106924314017988, 338.1823905601784759, 11.32908994701042538 ) ) ;
#682 = CARTESIAN_POINT ( 'NONE',  ( -11.93348319268872970, 440.6823905683721136, -3.332260488124732856 ) ) ;
#683 = VERTEX_POINT ( 'NONE', #12675 ) ;
#684 = CARTESIAN_POINT ( 'NONE',  ( 115.7989814974898337, 152.5259582928263740, -20.00000000000000355 ) ) ;
#685 = CARTESIAN_POINT ( 'NONE',  ( -22.27502019258947996, 290.7448905683720568, -15.47720386886985544 ) ) ;
#686 = AXIS2_PLACEMENT_3D ( 'NONE', #15275, #2176, #3783 ) ;
#687 = CARTESIAN_POINT ( 'NONE',  ( -42.88789093042843348, 386.3073905683720000, 9.489475012073734561 ) ) ;
#688 = CARTESIAN_POINT ( 'NONE',  ( -21.03221929538692336, 374.1198905601785327, -18.47759065022572855 ) ) ;
#689 = CARTESIAN_POINT ( 'NONE',  ( -11.73070664223726922, 517.9323905765655809, -11.32908994701042715 ) ) ;
#690 = CARTESIAN_POINT ( 'NONE',  ( -11.93348319268872615, 398.5573905683720568, 3.332260488124728415 ) ) ;
#691 = CARTESIAN_POINT ( 'NONE',  ( -11.93348319268870839, 240.0573905683720000, 3.332260488124728415 ) ) ;
#692 = CARTESIAN_POINT ( 'NONE',  ( -25.35362745456398770, 426.6823905683720568, 16.75240474999998952 ) ) ;
#693 = CARTESIAN_POINT ( 'NONE',  ( -14.54375231895776466, 345.7448905765655809, 14.14213562373094568 ) ) ;
#694 = CARTESIAN_POINT ( 'NONE',  ( 0.5805565836007611225, 3.752776749732563477, 6.500000000000000000 ) ) ;
#695 = CARTESIAN_POINT ( 'NONE',  ( -25.35362745456397704, 316.6823905683720000, 16.75240474999998952 ) ) ;
#696 = DIRECTION ( 'NONE',  ( 1.000000000000000000, 0.000000000000000000, 0.000000000000000000 ) ) ;
#697 = CARTESIAN_POINT ( 'NONE',  ( -45.43829269268872650, 485.3698905683720568, 0.000000000000000000 ) ) ;
#698 = FACE_OUTER_BOUND ( 'NONE', #4314, .T. ) ;
#699 = DIRECTION ( 'NONE',  ( -1.191790137725560488E-16, 1.000000000000000000, -0.000000000000000000 ) ) ;
#700 = DIRECTION ( 'NONE',  ( -0.000000000000000000, -0.000000000000000000, -1.000000000000000000 ) ) ;
#701 = ADVANCED_FACE ( 'NONE', ( #5959 ), #6064, .T. ) ;
#702 = CARTESIAN_POINT ( 'NONE',  ( -22.27502019258947996, 378.4948905683720000, 15.47720386886985189 ) ) ;
#703 = DIRECTION ( 'NONE',  ( 0.000000000000000000, -1.000000000000000000, 0.000000000000000000 ) ) ;
#704 = CARTESIAN_POINT ( 'NONE',  ( -48.68588794268872988, 517.5573905601784190, 3.978247347593168115 ) ) ;
#705 = CARTESIAN_POINT ( 'NONE',  ( -32.01814843081344719, 336.0573905683721136, 16.75240474999999307 ) ) ;
#706 = ORIENTED_EDGE ( 'NONE', *, *, #13101, .F. ) ;
#707 = CARTESIAN_POINT ( 'NONE',  ( -28.68588794268873343, 511.3698905683720000, -16.75240474999999307 ) ) ;
#708 = EDGE_LOOP ( 'NONE', ( #11246, #4754, #21207, #11052 ) ) ;
#709 = CARTESIAN_POINT ( 'NONE',  ( -42.53266943217990104, 223.9102039777116602, -9.520562566242684710 ) ) ;
#710 = CARTESIAN_POINT ( 'NONE',  ( 4.700000000000000178, 6.500000000000000888, 0.000000000000000000 ) ) ;
#711 = PLANE ( 'NONE',  #10698 ) ;
#712 = CARTESIAN_POINT ( 'NONE',  ( -45.64106924314020119, 521.0573905765656946, -11.32908994701042538 ) ) ;
#713 = CARTESIAN_POINT ( 'NONE',  ( -25.35362745456399480, 466.6823905683720000, 16.75240474999998952 ) ) ;
#714 = ORIENTED_EDGE ( 'NONE', *, *, #20644, .F. ) ;
#715 = CARTESIAN_POINT ( 'NONE',  ( -11.93348319268873503, 478.5573905683721136, 3.332260488124728859 ) ) ;
#716 = CARTESIAN_POINT ( 'NONE',  ( -28.68588794268869790, 249.7448905601784475, 19.99999999999999289 ) ) ;
#717 = EDGE_CURVE ( 'NONE', #20672, #5108, #13166, .T. ) ;
#718 =( GEOMETRIC_REPRESENTATION_CONTEXT ( 3 ) GLOBAL_UNCERTAINTY_ASSIGNED_CONTEXT ( ( #1876 ) ) GLOBAL_UNIT_ASSIGNED_CONTEXT ( ( #11259, #6284, #3052 ) ) REPRESENTATION_CONTEXT ( 'NONE', 'WORKASPACE' ) );
#719 = CARTESIAN_POINT ( 'NONE',  ( -48.68588794268871567, 402.3073905765655809, 3.978247347593168115 ) ) ;
#720 = CARTESIAN_POINT ( 'NONE',  ( -11.73070664223724258, 297.9323905765655809, -11.32908994701042538 ) ) ;
#721 = DIRECTION ( 'NONE',  ( 0.000000000000000000, 0.000000000000000000, 1.000000000000000000 ) ) ;
#722 = DIRECTION ( 'NONE',  ( 1.000000000000000000, 0.000000000000000000, 0.000000000000000000 ) ) ;
#723 = DIRECTION ( 'NONE',  ( 0.000000000000000000, -0.000000000000000000, -1.000000000000000000 ) ) ;
#724 = AXIS2_PLACEMENT_3D ( 'NONE', #8934, #10982, #3964 ) ;
#725 = CARTESIAN_POINT ( 'NONE',  ( -45.64106924314016567, 261.0573905765656377, -11.32908994701042538 ) ) ;
#726 = CARTESIAN_POINT ( 'NONE',  ( -14.54375231895775222, 240.9948905601784759, 14.14213562373094568 ) ) ;
#727 = FACE_OUTER_BOUND ( 'NONE', #18825, .T. ) ;
#728 = CLOSED_SHELL ( 'NONE', ( #4202, #18729, #7183, #1313, #6098, #14803, #2877, #2308, #8698, #9259, #1514, #21123, #2681, #8425, #4950, #3532, #389, #2715, #19260, #14653, #15130, #14125, #19463, #13734, #19883, #19785, #7149, #16387, #12129, #10656, #9205, #12272, #16233, #3470, #2143, #15969, #3158, #11966, #8090, #20749, #11190, #649, #18699, #8016, #5574, #907, #20543, #1966, #6567, #13747, #21117, #1097, #12190, #73, #11691, #16866, #10538, #19874, #8200, #12587, #9693, #14131, #2231, #11601, #7880, #15316, #13856, #1907, #10138, #3997, #11879, #20146, #15364, #1047, #17279, #12993, #4417, #13206, #9791, #6710, #19859, #8106, #17682, #4283, #12076, #13479, #20733, #20323, #20863, #3939, #1701, #7829, #2906, #15283, #6218, #20450, #19796, #1639, #4404, #10989, #20740, #14224, #2354, #839, #7752, #14892, #15777, #1840, #3193, #15792, #9164, #1436, #7801, #12477, #8633, #18193, #14455, #9085, #11057 ) ) ;
#729 = CARTESIAN_POINT ( 'NONE',  ( -28.68588794268870501, 282.8698905683720568, -16.75240474999999307 ) ) ;
#730 = EDGE_CURVE ( 'NONE', #15685, #3984, #3339, .T. ) ;
#731 = CARTESIAN_POINT ( 'NONE',  ( -40.01497788969912506, 255.6823905601785043, -16.95518130045146421 ) ) ;
#732 = CARTESIAN_POINT ( 'NONE',  ( -21.03221929538691626, 405.1198905765656377, 18.47759065022572500 ) ) ;
#733 = EDGE_CURVE ( 'NONE', #15687, #8097, #12465, .T. ) ;
#734 = CARTESIAN_POINT ( 'NONE',  ( -16.84014894278200103, 451.6198905683720568, -11.84573899990672707 ) ) ;
#735 = CARTESIAN_POINT ( 'NONE',  ( -24.70764059509555466, 329.1823905765656377, -19.99999999999999289 ) ) ;
#736 = CARTESIAN_POINT ( 'NONE',  ( -14.48388495494898720, 261.3073905683720568, -9.489475012073736337 ) ) ;
#737 = ORIENTED_EDGE ( 'NONE', *, *, #646, .T. ) ;
#738 = CARTESIAN_POINT ( 'NONE',  ( -14.54375231895775755, 248.2448905765656377, -14.14213562373094746 ) ) ;
#739 = VERTEX_POINT ( 'NONE', #17751 ) ;
#740 = CARTESIAN_POINT ( 'NONE',  ( -22.27502019258950128, 492.2448905683720000, -15.47720386886985544 ) ) ;
#741 = AXIS2_PLACEMENT_3D ( 'NONE', #1558, #4786, #9334 ) ;
#742 = VECTOR ( 'NONE', #9615, 1000.000000000000114 ) ;
#743 = EDGE_LOOP ( 'NONE', ( #12218, #10443, #10130, #5735 ) ) ;
#744 = DIRECTION ( 'NONE',  ( -0.8090169943749474513, 0.000000000000000000, -0.5877852522924730261 ) ) ;
#745 = CARTESIAN_POINT ( 'NONE',  ( -38.17536295476244135, 242.3073905683720284, -14.20200298773971426 ) ) ;
#746 = ORIENTED_EDGE ( 'NONE', *, *, #17623, .T. ) ;
#747 = CARTESIAN_POINT ( 'NONE',  ( -48.68588794268873698, 573.2448905601785327, 0.000000000000000000 ) ) ;
#748 = CARTESIAN_POINT ( 'NONE',  ( -11.73070664223725856, 456.0573905765655809, 11.32908994701042005 ) ) ;
#749 = CARTESIAN_POINT ( 'NONE',  ( -48.68588794268870146, 327.2448905601785327, 0.000000000000000000 ) ) ;
#750 = CARTESIAN_POINT ( 'NONE',  ( 158.8141120573112630, 628.3356379279406383, 0.000000000000000000 ) ) ;
#751 = CARTESIAN_POINT ( 'NONE',  ( 14.09825962131072785, 160.1716627696692683, 49.99999999999999289 ) ) ;
#752 =( BOUNDED_CURVE ( )  B_SPLINE_CURVE ( 2, ( #12930, #11188, #17789, #4383, #17577, #16290, #7615, #7827, #20932, #11078, #9665, #14457, #2981, #9461, #1357, #7929, #14560 ),
 .UNSPECIFIED., .F., .T. ) 
 B_SPLINE_CURVE_WITH_KNOTS ( ( 3, 2, 2, 2, 2, 2, 2, 2, 3 ),
 ( 0.8750000000000002220, 0.8769531250000002220, 0.8789062500000002220, 0.8808593750000002220, 0.8828125000000002220, 0.8847656250000002220, 0.8867187500000002220, 0.8886718750000002220, 0.8906250000000002220 ),
 .UNSPECIFIED. ) 
 CURVE ( )  GEOMETRIC_REPRESENTATION_ITEM ( )  RATIONAL_B_SPLINE_CURVE ( ( 0.9999999999999977796, 0.9807852804032326510, 1.000000000000000000, 0.9807852804032304306, 1.000000000000000000, 0.9807852804032304306, 1.000000000000000000, 0.9807852804032304306, 1.000000000000000000, 0.9807852804032304306, 1.000000000000000000, 0.9807852804032304306, 1.000000000000000000, 0.9807852804032304306, 1.000000000000000000, 0.9807852804032282101, 1.000000000000002220 ) ) 
 REPRESENTATION_ITEM ( '' )  );
#753 = CARTESIAN_POINT ( 'NONE',  ( -13.20868407381887799, 519.7448905683720568, 6.410867750099229490 ) ) ;
#754 = CARTESIAN_POINT ( 'NONE',  ( 52.94681837068318941, 78.74778544605769071, -94.99999999999994316 ) ) ;
#755 = CARTESIAN_POINT ( 'NONE',  ( -38.17536295476243424, 255.4323905683720284, 14.20200298773971781 ) ) ;
#756 = CARTESIAN_POINT ( 'NONE',  ( -44.16309181155856578, 335.9948905683720000, 6.410867750099241924 ) ) ;
#757 = CARTESIAN_POINT ( 'NONE',  ( -42.82802356641965247, 318.4948905601784759, 14.14213562373094923 ) ) ;
#758 = AXIS2_PLACEMENT_3D ( 'NONE', #6274, #19685, #17847 ) ;
#759 = CARTESIAN_POINT ( 'NONE',  ( -28.68588794268870501, 304.4948905765656377, 19.99999999999999289 ) ) ;
#760 = CARTESIAN_POINT ( 'NONE',  ( -14.48388495494900496, 399.8073905683720568, -9.489475012073736337 ) ) ;
#761 = CARTESIAN_POINT ( 'NONE',  ( -48.68588794268887199, 322.3073905765654672, 3.978247347592742678 ) ) ;
#762 = CARTESIAN_POINT ( 'NONE',  ( -40.01497788969913216, 388.8073905601784759, 16.95518130045146776 ) ) ;
#763 = VERTEX_POINT ( 'NONE', #10929 ) ;
#764 = CARTESIAN_POINT ( 'NONE',  ( 292.4526463419396691, 308.2087638784415162, 20.00000000000000355 ) ) ;
#765 = ORIENTED_EDGE ( 'NONE', *, *, #15458, .T. ) ;
#766 = ORIENTED_EDGE ( 'NONE', *, *, #15273, .F. ) ;
#767 = CARTESIAN_POINT ( 'NONE',  ( -40.53162694259545162, 504.1198905683720568, -11.84573899990672707 ) ) ;
#768 = DIRECTION ( 'NONE',  ( 0.000000000000000000, 0.000000000000000000, -1.000000000000000000 ) ) ;
#769 = ORIENTED_EDGE ( 'NONE', *, *, #17344, .T. ) ;
#770 = CARTESIAN_POINT ( 'NONE',  ( -32.01814843081344009, 307.5573905683719431, 16.75240474999999307 ) ) ;
#771 = AXIS2_PLACEMENT_3D ( 'NONE', #5394, #18697, #1965 ) ;
#772 = ORIENTED_EDGE ( 'NONE', *, *, #7755, .F. ) ;
#773 = CARTESIAN_POINT ( 'NONE',  ( -45.43829269268870519, 344.1823905683719431, 3.332260488124734632 ) ) ;
#774 = EDGE_CURVE ( 'NONE', #19077, #15843, #2641, .T. ) ;
#775 = VECTOR ( 'NONE', #5701, 1000.000000000000000 ) ;
#776 = CARTESIAN_POINT ( 'NONE',  ( -40.53162694259543741, 345.1198905683720568, 11.84573899990672885 ) ) ;
#777 = EDGE_CURVE ( 'NONE', #1912, #13157, #11419, .T. ) ;
#778 = CARTESIAN_POINT ( 'NONE',  ( -24.70764059509555111, 279.1823905765656377, -19.99999999999999289 ) ) ;
#779 = DIRECTION ( 'NONE',  ( 0.000000000000000000, -1.000000000000000000, 0.000000000000000000 ) ) ;
#780 = CARTESIAN_POINT ( 'NONE',  ( -25.35362745456397704, 251.0573905683720000, -16.75240474999999307 ) ) ;
#781 = CARTESIAN_POINT ( 'NONE',  ( -36.33955658999052929, 463.8698905765656377, 18.47759065022572500 ) ) ;
#782 = CARTESIAN_POINT ( 'NONE',  ( -25.35362745456399480, 402.5573905683720000, -16.75240474999999307 ) ) ;
#783 = CARTESIAN_POINT ( 'NONE',  ( -5.502341142637721561, 600.7448905601785327, -7.573322868991255952 ) ) ;
#784 = CARTESIAN_POINT ( 'NONE',  ( -8.685887942688632180, 352.5573905601784759, -3.978247347592952732 ) ) ;
#785 = PRODUCT_DEFINITION_CONTEXT ( 'detailed design', #9294, 'design' ) ;
#786 = CARTESIAN_POINT ( 'NONE',  ( -28.68588794268873343, 509.4948905765655809, -19.99999999999999289 ) ) ;
#787 = ADVANCED_FACE ( 'NONE', ( #19771 ), #9521, .T. ) ;
#788 = CARTESIAN_POINT ( 'NONE',  ( -44.16309181155857999, 454.4948905683720568, 6.410867750099241924 ) ) ;
#789 = ORIENTED_EDGE ( 'NONE', *, *, #4805, .T. ) ;
#790 = AXIS2_PLACEMENT_3D ( 'NONE', #4343, #10924, #17535 ) ;
#791 = CARTESIAN_POINT ( 'NONE',  ( -32.66413529028188378, 449.4323905601785327, 19.99999999999999289 ) ) ;
#792 = CARTESIAN_POINT ( 'NONE',  ( -22.27502019258946930, 286.9948905683720000, 15.47720386886985189 ) ) ;
#793 = ORIENTED_EDGE ( 'NONE', *, *, #1569, .T. ) ;
#794 = ORIENTED_EDGE ( 'NONE', *, *, #7092, .F. ) ;
#795 = VERTEX_POINT ( 'NONE', #9310 ) ;
#796 = LINE ( 'NONE', #2405, #6289 ) ;
#797 = CARTESIAN_POINT ( 'NONE',  ( -38.17536295476244135, 305.4323905683720000, 14.20200298773971781 ) ) ;
#798 = CARTESIAN_POINT ( 'NONE',  ( -35.09675569278794427, 373.4948905683720568, -15.47720386886985544 ) ) ;
#799 = CARTESIAN_POINT ( 'NONE',  ( -36.33955658999050797, 375.3698905601784759, -18.47759065022572855 ) ) ;
#800 = CARTESIAN_POINT ( 'NONE',  ( -10.20829729246300488, 516.3698905765656946, 7.653668647301790529 ) ) ;
#801 = CARTESIAN_POINT ( 'NONE',  ( -25.35362745456399836, 411.0573905683720568, -16.75240474999999307 ) ) ;
#802 = CARTESIAN_POINT ( 'NONE',  ( -11.93348319268870839, 240.6823905683720284, -3.332260488124732856 ) ) ;
#803 = AXIS2_PLACEMENT_3D ( 'NONE', #18452, #8919, #7182 ) ;
#804 = CARTESIAN_POINT ( 'NONE',  ( -32.01814843081344719, 411.6823905683720000, -16.75240474999999307 ) ) ;
#805 = CARTESIAN_POINT ( 'NONE',  ( -47.16347859291444422, 351.3698905765655809, -7.653668647301793193 ) ) ;
#806 = DIRECTION ( 'NONE',  ( -0.000000000000000000, -0.000000000000000000, 1.000000000000000000 ) ) ;
#807 = CARTESIAN_POINT ( 'NONE',  ( -16.84014894278197971, 297.6198905683720000, 11.84573899990672530 ) ) ;
#808 = CARTESIAN_POINT ( 'NONE',  ( 0.000000000000000000, 0.000000000000000000, 0.000000000000000000 ) ) ;
#809 = CARTESIAN_POINT ( 'NONE',  ( -11.93348319268873325, 460.0573905683720568, 3.332260488124728415 ) ) ;
#810 = CARTESIAN_POINT ( 'NONE',  ( -28.68588794268874054, 573.2448905601785327, 0.000000000000000000 ) ) ;
#811 = CARTESIAN_POINT ( 'NONE',  ( -43.67482055103364047, 200.1767183643995054, -0.6599055232175776720 ) ) ;
#812 = CARTESIAN_POINT ( 'NONE',  ( -14.54375231895775045, 225.7448905765656093, 14.14213562373094568 ) ) ;
#813 = CARTESIAN_POINT ( 'NONE',  ( -32.01814843081344719, 367.5573905683721136, 16.75240474999999307 ) ) ;
#814 = CARTESIAN_POINT ( 'NONE',  ( -33.24036626417445461, 53.08430543508956134, -120.4996691248974656 ) ) ;
#815 = CIRCLE ( 'NONE', #18408, 50.00000000000000000 ) ;
#816 = CARTESIAN_POINT ( 'NONE',  ( -42.82802356641968089, 535.9948905601785327, -14.14213562373094746 ) ) ;
#817 = CARTESIAN_POINT ( 'NONE',  ( -16.84014894278198327, 337.6198905683720000, 11.84573899990672530 ) ) ;
#818 = ORIENTED_EDGE ( 'NONE', *, *, #12595, .F. ) ;
#819 = CARTESIAN_POINT ( 'NONE',  ( -44.16309181155859420, 513.2448905683719431, -6.410867750099231266 ) ) ;
#820 = ORIENTED_EDGE ( 'NONE', *, *, #20266, .T. ) ;
#821 = CARTESIAN_POINT ( 'NONE',  ( -42.82802356641965957, 355.9948905601784759, -14.14213562373094746 ) ) ;
#822 = CARTESIAN_POINT ( 'NONE',  ( -45.30451366577094063, 223.9102039777116033, -2.213613569785925606 ) ) ;
#823 = CARTESIAN_POINT ( 'NONE',  ( -18.81370552131603091, 600.7448905601785327, 6.112943483001358480 ) ) ;
#824 = CARTESIAN_POINT ( 'NONE',  ( -49.57497958038186425, 230.5765313837437418, 60.00000000000000000 ) ) ;
#825 = CARTESIAN_POINT ( 'NONE',  ( -8.685887942688422569, 517.3073905765655809, -3.978247347592394068 ) ) ;
#826 = CARTESIAN_POINT ( 'NONE',  ( -25.35362745456400191, 461.0573905683721136, -16.75240474999999307 ) ) ;
#827 = VERTEX_POINT ( 'NONE', #16139 ) ;
#828 = CARTESIAN_POINT ( 'NONE',  ( -35.09675569278796559, 465.7448905683720568, 15.47720386886985366 ) ) ;
#829 = CARTESIAN_POINT ( 'NONE',  ( -21.03221929538689849, 245.1198905765656377, 18.47759065022572500 ) ) ;
#830 = VECTOR ( 'NONE', #8957, 1000.000000000000000 ) ;
#831 = CARTESIAN_POINT ( 'NONE',  ( -36.33955658999051508, 410.1198905765656377, -18.47759065022572855 ) ) ;
#832 = DIRECTION ( 'NONE',  ( 0.000000000000000000, 1.000000000000000000, -0.000000000000000000 ) ) ;
#833 = DIRECTION ( 'NONE',  ( -1.000000000000000000, 0.000000000000000000, 0.000000000000000000 ) ) ;
#834 = DIRECTION ( 'NONE',  ( 1.000000000000000000, 0.000000000000000000, 0.000000000000000000 ) ) ;
#835 = CARTESIAN_POINT ( 'NONE',  ( 6.416697501590670427, 172.9933428177121471, -60.00000000000000000 ) ) ;
#836 = CIRCLE ( 'NONE', #10824, 21.20245194746113526 ) ;
#837 = CARTESIAN_POINT ( 'NONE',  ( -48.68588794268869435, 261.9948905765655809, 0.000000000000000000 ) ) ;
#838 = CARTESIAN_POINT ( 'NONE',  ( -24.70764059509553334, 240.0573905601785043, 19.99999999999998934 ) ) ;
#839 = ADVANCED_FACE ( 'NONE', ( #6238 ), #6566, .T. ) ;
#840 = CARTESIAN_POINT ( 'NONE',  ( 6.416697501590670427, 217.7548513357008630, 49.99999999999999289 ) ) ;
#841 = CARTESIAN_POINT ( 'NONE',  ( -42.88789093042842637, 284.4323905683720000, -9.489475012073736337 ) ) ;
#842 = CARTESIAN_POINT ( 'NONE',  ( -28.68588794268872633, 452.8698905683720000, -16.75240474999999307 ) ) ;
#843 = CARTESIAN_POINT ( 'NONE',  ( -28.68588794268871212, 329.4948905765656377, -19.99999999999999289 ) ) ;
#844 = CARTESIAN_POINT ( 'NONE',  ( -45.43829269268869098, 265.0573905683720568, -3.332260488124726194 ) ) ;
#845 = ORIENTED_EDGE ( 'NONE', *, *, #11128, .T. ) ;
#846 = LINE ( 'NONE', #7519, #3923 ) ;
#847 = ORIENTED_EDGE ( 'NONE', *, *, #2670, .F. ) ;
#848 = CARTESIAN_POINT ( 'NONE',  ( -19.19641293061499354, 478.8073905683720568, 14.20200298773971426 ) ) ;
#849 = AXIS2_PLACEMENT_3D ( 'NONE', #5042, #1929, #16634 ) ;
#850 = ORIENTED_EDGE ( 'NONE', *, *, #4862, .F. ) ;
#851 = CARTESIAN_POINT ( 'NONE',  ( 105.7989814974898479, 152.5259582928263740, 20.00000000000000355 ) ) ;
#852 = CARTESIAN_POINT ( 'NONE',  ( -22.27502019258946220, 236.9948905683720284, 15.47720386886985189 ) ) ;
#853 = ORIENTED_EDGE ( 'NONE', *, *, #17633, .T. ) ;
#854 = DIRECTION ( 'NONE',  ( -1.000000000000000000, -0.000000000000000000, -0.000000000000000000 ) ) ;
#855 = ADVANCED_FACE ( 'NONE', ( #12574 ), #17645, .F. ) ;
#856 = CARTESIAN_POINT ( 'NONE',  ( -10.20829729246299777, 466.3698905765656377, 7.653668647301790529 ) ) ;
#857 = FACE_OUTER_BOUND ( 'NONE', #9920, .T. ) ;
#858 = CARTESIAN_POINT ( 'NONE',  ( -28.68588794268872277, 174.3162933293988033, -20.00000000000000000 ) ) ;
#859 = CARTESIAN_POINT ( 'NONE',  ( -32.01814843081343298, 233.1823905683720284, -16.75240474999999307 ) ) ;
#860 = CARTESIAN_POINT ( 'NONE',  ( -13.20868407381887977, 520.9948905683720568, -6.410867750099233042 ) ) ;
#861 = DIRECTION ( 'NONE',  ( 0.000000000000000000, -1.000000000000000000, 0.000000000000000000 ) ) ;
#862 = DIRECTION ( 'NONE',  ( 1.000000000000000000, 0.000000000000000000, 0.000000000000000000 ) ) ;
#863 = CARTESIAN_POINT ( 'NONE',  ( -13.20868407381884779, 239.4948905683720284, -6.410867750099233042 ) ) ;
#864 = CARTESIAN_POINT ( 'NONE',  ( -11.93348319268871727, 330.3698905683720000, -2.051577885510841163E-15 ) ) ;
#865 = DIRECTION ( 'NONE',  ( -0.000000000000000000, -0.000000000000000000, -1.000000000000000000 ) ) ;
#866 = CARTESIAN_POINT ( 'NONE',  ( -1.025382690249028173, 213.9102039777116602, -25.00000000000000000 ) ) ;
#867 = EDGE_CURVE ( 'NONE', #17801, #4217, #13526, .T. ) ;
#868 = CARTESIAN_POINT ( 'NONE',  ( -32.01814843081345430, 391.6823905683720568, -16.75240474999999307 ) ) ;
#869 = CARTESIAN_POINT ( 'NONE',  ( -40.53162694259545873, 534.1198905683720568, -11.84573899990672707 ) ) ;
#870 = CARTESIAN_POINT ( 'NONE',  ( -42.82802356641965957, 385.9948905601784759, -14.14213562373094746 ) ) ;
#871 = ORIENTED_EDGE ( 'NONE', *, *, #21201, .F. ) ;
#872 = FACE_OUTER_BOUND ( 'NONE', #15854, .T. ) ;
#873 = ORIENTED_EDGE ( 'NONE', *, *, #38, .F. ) ;
#874 = EDGE_LOOP ( 'NONE', ( #5710, #13740, #20222, #9194 ) ) ;
#875 = CARTESIAN_POINT ( 'NONE',  ( -22.27502019258949417, 508.4948905683720568, 15.47720386886985189 ) ) ;
#876 = CARTESIAN_POINT ( 'NONE',  ( -48.68588794268879383, 292.3073905765656377, 3.978247347592954952 ) ) ;
#877 = EDGE_LOOP ( 'NONE', ( #2483, #11, #10820, #14178 ) ) ;
#878 = EDGE_CURVE ( 'NONE', #5613, #19077, #11132, .T. ) ;
#879 = CARTESIAN_POINT ( 'NONE',  ( -22.27502019258946930, 308.4948905683720568, 15.47720386886985189 ) ) ;
#880 = VERTEX_POINT ( 'NONE', #1839 ) ;
#881 = CARTESIAN_POINT ( 'NONE',  ( -38.17536295476244845, 335.4323905683720000, 14.20200298773971781 ) ) ;
#882 = CARTESIAN_POINT ( 'NONE',  ( -19.19641293061497578, 337.3073905683720568, 14.20200298773971426 ) ) ;
#883 = CARTESIAN_POINT ( 'NONE',  ( -8.685887942688712116, 276.6823905765655809, 3.978247347593161010 ) ) ;
#884 = PLANE ( 'NONE',  #19670 ) ;
#885 = CARTESIAN_POINT ( 'NONE',  ( -11.93348319268870661, 238.5573905683720284, 3.332260488124728859 ) ) ;
#886 = CARTESIAN_POINT ( 'NONE',  ( -43.52298375438361688, 200.6544955639567149, 2.225641045960682796 ) ) ;
#887 = APPLICATION_CONTEXT ( 'automotive_design' ) ;
#888 = CARTESIAN_POINT ( 'NONE',  ( -45.43829269268871229, 395.0573905683719431, -3.332260488124726194 ) ) ;
#889 = LINE ( 'NONE', #9296, #7146 ) ;
#890 = DIRECTION ( 'NONE',  ( 0.000000000000000000, 1.000000000000000000, -0.000000000000000000 ) ) ;
#891 = CARTESIAN_POINT ( 'NONE',  ( -14.54375231895778775, 508.2448905765656377, -14.14213562373094746 ) ) ;
#892 = CARTESIAN_POINT ( 'NONE',  ( -35.09675569278795848, 435.7448905683720000, 15.47720386886985366 ) ) ;
#893 = EDGE_LOOP ( 'NONE', ( #12, #19288 ) ) ;
#894 = CARTESIAN_POINT ( 'NONE',  ( -17.35679799567830983, 443.8073905601784759, -16.95518130045146421 ) ) ;
#895 = ORIENTED_EDGE ( 'NONE', *, *, #3138, .F. ) ;
#896 = LINE ( 'NONE', #14196, #5632 ) ;
#897 = ORIENTED_EDGE ( 'NONE', *, *, #15663, .F. ) ;
#898 = ORIENTED_EDGE ( 'NONE', *, *, #6988, .F. ) ;
#899 = LINE ( 'NONE', #11030, #10091 ) ;
#900 = CARTESIAN_POINT ( 'NONE',  ( -28.68588794268870856, 329.7448905601784759, 19.99999999999999289 ) ) ;
#901 = CARTESIAN_POINT ( 'NONE',  ( -11.93348319268871549, 299.1823905683720000, -3.332260488124732856 ) ) ;
#902 = CARTESIAN_POINT ( 'NONE',  ( -25.35362745456398059, 368.1823905683721136, 16.75240474999998952 ) ) ;
#903 = CARTESIAN_POINT ( 'NONE',  ( -8.685887942688724550, 372.2448905601784759, -2.449293598294705724E-15 ) ) ;
#904 = CARTESIAN_POINT ( 'NONE',  ( -11.73070664223726745, 526.0573905765656946, 11.32908994701042005 ) ) ;
#905 = CARTESIAN_POINT ( 'NONE',  ( -16.84014894278199392, 407.6198905683720568, 11.84573899990672530 ) ) ;
#906 = CARTESIAN_POINT ( 'NONE',  ( -13.20868407381884602, 230.9948905683720284, -6.410867750099233042 ) ) ;
#907 = ADVANCED_FACE ( 'NONE', ( #11663 ), #10238, .F. ) ;
#908 = CARTESIAN_POINT ( 'NONE',  ( -25.35362745456399836, 411.0573905683720568, -16.75240474999999307 ) ) ;
#909 = ITEM_DEFINED_TRANSFORMATION ( 'NONE', 'NONE', #5885,  #12794 ) ;
#910 = EDGE_CURVE ( 'NONE', #13843, #4925, #3656, .T. ) ;
#911 = CARTESIAN_POINT ( 'NONE',  ( -36.33955658999050797, 340.1198905765655809, -18.47759065022572855 ) ) ;
#912 = DIRECTION ( 'NONE',  ( -0.02112707654195870172, 0.9250389998264586522, -0.3792841882241536067 ) ) ;
#913 = CARTESIAN_POINT ( 'NONE',  ( -44.16309181155855867, 314.4948905683720000, 6.410867750099241924 ) ) ;
#914 =( NAMED_UNIT ( * ) PLANE_ANGLE_UNIT ( ) SI_UNIT ( $, .RADIAN. ) );
#915 = CARTESIAN_POINT ( 'NONE',  ( -32.01814843081346140, 467.5573905683721136, 16.75240474999999307 ) ) ;
#916 = CARTESIAN_POINT ( 'NONE',  ( -24.70764059509556532, 514.8073905765656946, 19.99999999999998934 ) ) ;
#917 = DIRECTION ( 'NONE',  ( 0.000000000000000000, 1.000000000000000000, -0.000000000000000000 ) ) ;
#918 = PLANE ( 'NONE',  #7806 ) ;
#919 = ADVANCED_FACE ( 'NONE', ( #6784 ), #8728, .T. ) ;
#920 = CARTESIAN_POINT ( 'NONE',  ( -35.09675569278795138, 367.2448905683720000, 15.47720386886985366 ) ) ;
#921 = CARTESIAN_POINT ( 'NONE',  ( -47.16347859291445843, 506.6198905601784190, -7.653668647301793193 ) ) ;
#922 = CARTESIAN_POINT ( 'NONE',  ( -45.43829269268870519, 344.1823905683719431, 3.332260488124734632 ) ) ;
#923 = EDGE_CURVE ( 'NONE', #13560, #11943, #3445, .T. ) ;
#924 = CIRCLE ( 'NONE', #10232, 6.500000000000000888 ) ;
#925 = ORIENTED_EDGE ( 'NONE', *, *, #2214, .F. ) ;
#926 = CARTESIAN_POINT ( 'NONE',  ( -45.43829269268872650, 503.8698905683720568, 0.000000000000000000 ) ) ;
#927 = ORIENTED_EDGE ( 'NONE', *, *, #15522, .T. ) ;
#928 = DIRECTION ( 'NONE',  ( 0.000000000000000000, -1.000000000000000000, 0.000000000000000000 ) ) ;
#929 = CARTESIAN_POINT ( 'NONE',  ( -13.20868407381886556, 419.7448905683720000, 6.410867750099229490 ) ) ;
#930 = CARTESIAN_POINT ( 'NONE',  ( -47.16347859291443712, 291.3698905765655809, -7.653668647301793193 ) ) ;
#931 = CYLINDRICAL_SURFACE ( 'NONE', #21088, 125.0000000000000000 ) ;
#932 = CARTESIAN_POINT ( 'NONE',  ( -44.16309181155858710, 473.2448905683720568, -6.410867750099231266 ) ) ;
#933 = ORIENTED_EDGE ( 'NONE', *, *, #17134, .T. ) ;
#934 = CARTESIAN_POINT ( 'NONE',  ( -14.48388495494901029, 467.9323905683721136, 9.489475012073731008 ) ) ;
#935 = CARTESIAN_POINT ( 'NONE',  ( -45.64106924314016567, 242.9323905765656377, 11.32908994701042538 ) ) ;
#936 = CARTESIAN_POINT ( 'NONE',  ( -24.70764059509555821, 404.8073905765656377, 19.99999999999998934 ) ) ;
#937 = FACE_OUTER_BOUND ( 'NONE', #6121, .T. ) ;
#938 = CARTESIAN_POINT ( 'NONE',  ( -28.68588794268871567, 369.4948905765656377, -19.99999999999999289 ) ) ;
#939 = CARTESIAN_POINT ( 'NONE',  ( 79.78925230247502043, 142.5259582928263455, -40.00000000000000000 ) ) ;
#940 = CARTESIAN_POINT ( 'NONE',  ( 20.42502041961813930, 230.5765313837437418, 60.00000000000000000 ) ) ;
#941 = VECTOR ( 'NONE', #20908, 1000.000000000000000 ) ;
#942 = CARTESIAN_POINT ( 'NONE',  ( -28.68588794268874409, 600.7448905601785327, 0.000000000000000000 ) ) ;
#943 = CARTESIAN_POINT ( 'NONE',  ( -8.685887942688799157, 241.9323905601784475, 3.978247347593374172 ) ) ;
#944 = CARTESIAN_POINT ( 'NONE',  ( -35.86044580198795018, 223.9104597372275123, 18.66884633871304899 ) ) ;
#945 = CARTESIAN_POINT ( 'NONE',  ( -16.84014894278197971, 281.6198905683720000, -11.84573899990672707 ) ) ;
#946 = CARTESIAN_POINT ( 'NONE',  ( -28.68588794268870146, 244.7448905601785043, -19.99999999999999289 ) ) ;
#947 = VECTOR ( 'NONE', #1680, 1000.000000000000114 ) ;
#948 = DIRECTION ( 'NONE',  ( 0.000000000000000000, -1.000000000000000000, 0.000000000000000000 ) ) ;
#949 = CARTESIAN_POINT ( 'NONE',  ( -40.53162694259544452, 434.1198905683720000, -11.84573899990672707 ) ) ;
#950 = DIRECTION ( 'NONE',  ( 0.000000000000000000, -1.000000000000000000, 0.000000000000000000 ) ) ;
#951 = CARTESIAN_POINT ( 'NONE',  ( -13.20868407381884779, 250.9948905683720284, -6.410867750099233042 ) ) ;
#952 = VERTEX_POINT ( 'NONE', #10343 ) ;
#953 = LINE ( 'NONE', #10873, #17064 ) ;
#954 = ORIENTED_EDGE ( 'NONE', *, *, #14883, .F. ) ;
#955 = CARTESIAN_POINT ( 'NONE',  ( -40.53162694259545162, 486.6198905683720000, 11.84573899990672885 ) ) ;
#956 = AXIS2_PLACEMENT_3D ( 'NONE', #2213, #8797, #5337 ) ;
#957 = ORIENTED_EDGE ( 'NONE', *, *, #6491, .T. ) ;
#958 = EDGE_CURVE ( 'NONE', #16482, #2272, #637, .T. ) ;
#959 = DIRECTION ( 'NONE',  ( 0.000000000000000000, 0.000000000000000000, -1.000000000000000000 ) ) ;
#960 = CARTESIAN_POINT ( 'NONE',  ( -14.48388495494898542, 239.8073905683720284, -9.489475012073736337 ) ) ;
#961 = EDGE_LOOP ( 'NONE', ( #6161, #9124, #13988, #14252 ) ) ;
#962 = DIRECTION ( 'NONE',  ( 0.000000000000000000, 0.000000000000000000, 1.000000000000000000 ) ) ;
#963 = AXIS2_PLACEMENT_3D ( 'NONE', #5944, #6051, #12561 ) ;
#964 = CARTESIAN_POINT ( 'NONE',  ( -17.35679799567830628, 465.4323905765656946, 16.95518130045146421 ) ) ;
#965 = PRODUCT_DEFINITION_SHAPE ( 'NONE', 'NONE',  #5449 ) ;
#966 = CARTESIAN_POINT ( 'NONE',  ( -8.685887942688713892, 286.9948905765656377, -2.449293598294705724E-15 ) ) ;
#967 = CARTESIAN_POINT ( 'NONE',  ( -26.23092855549762348, 223.9102039777116318, -18.75754572640088114 ) ) ;
#968 = CARTESIAN_POINT ( 'NONE',  ( -42.88789093042841927, 226.3073905683720000, 9.489475012073734561 ) ) ;
#969 = CARTESIAN_POINT ( 'NONE',  ( -25.35362745456400901, 512.5573905683719431, -16.75240474999999307 ) ) ;
#970 = DIRECTION ( 'NONE',  ( 0.000000000000000000, -1.000000000000000000, 0.000000000000000000 ) ) ;
#971 = CARTESIAN_POINT ( 'NONE',  ( -40.53162694259542320, 255.1198905683720284, 11.84573899990672885 ) ) ;
#972 = CARTESIAN_POINT ( 'NONE',  ( -35.09675569278795138, 337.2448905683720568, 15.47720386886985366 ) ) ;
#973 = AXIS2_PLACEMENT_3D ( 'NONE', #2028, #2337, #11954 ) ;
#974 = CARTESIAN_POINT ( 'NONE',  ( -28.68588794268872633, 469.7448905601784759, 19.99999999999999289 ) ) ;
#975 = CARTESIAN_POINT ( 'NONE',  ( -48.68588794268870856, 357.2448905601784759, 0.000000000000000000 ) ) ;
#976 = ADVANCED_FACE ( 'NONE', ( #10029 ), #11976, .T. ) ;
#977 = VECTOR ( 'NONE', #2716, 1000.000000000000114 ) ;
#978 = CARTESIAN_POINT ( 'NONE',  ( -40.53162694259544452, 392.6198905683720568, -11.84573899990672707 ) ) ;
#979 = CARTESIAN_POINT ( 'NONE',  ( 158.8141120573112630, 610.7448905601785327, 10.00000000000000888 ) ) ;
#980 = CARTESIAN_POINT ( 'NONE',  ( -45.64106924314018698, 378.1823905601785327, 11.32908994701042715 ) ) ;
#981 = ORIENTED_EDGE ( 'NONE', *, *, #5565, .T. ) ;
#982 = CARTESIAN_POINT ( 'NONE',  ( -8.685887942688726326, 402.2448905601784759, -2.449293598294705724E-15 ) ) ;
#983 = VERTEX_POINT ( 'NONE', #16655 ) ;
#984 = VERTEX_POINT ( 'NONE', #12082 ) ;
#985 = CARTESIAN_POINT ( 'NONE',  ( -19.19641293061499709, 498.8073905683720000, 14.20200298773971426 ) ) ;
#986 = CARTESIAN_POINT ( 'NONE',  ( -28.68588794268870501, 294.4948905765656377, 19.99999999999999289 ) ) ;
#987 = ORIENTED_EDGE ( 'NONE', *, *, #20806, .F. ) ;
#988 = CARTESIAN_POINT ( 'NONE',  ( -28.68588794268870856, 302.8698905683720000, -16.75240474999999307 ) ) ;
#989 = ORIENTED_EDGE ( 'NONE', *, *, #1574, .T. ) ;
#990 = CARTESIAN_POINT ( 'NONE',  ( -45.43829269268870519, 333.5573905683720568, -3.332260488124726194 ) ) ;
#991 = CARTESIAN_POINT ( 'NONE',  ( -25.35362745456398059, 346.6823905683720568, 16.75240474999998952 ) ) ;
#992 = EDGE_CURVE ( 'NONE', #17870, #16862, #20206, .T. ) ;
#993 = CARTESIAN_POINT ( 'NONE',  ( -24.70764059509553690, 274.8073905765656377, 19.99999999999998934 ) ) ;
#994 = CARTESIAN_POINT ( 'NONE',  ( -32.66413529028188378, 499.8073905765655809, -19.99999999999999289 ) ) ;
#995 = CARTESIAN_POINT ( 'NONE',  ( -14.48388495494898365, 247.9323905683720568, 9.489475012073731008 ) ) ;
#996 = CARTESIAN_POINT ( 'NONE',  ( -11.93348319268872615, 400.0573905683720568, 3.332260488124728415 ) ) ;
#997 = CARTESIAN_POINT ( 'NONE',  ( 28.16023193154655502, 323.8848358243226357, 40.00000000000000000 ) ) ;
#998 = DIRECTION ( 'NONE',  ( -1.374938938973709817E-16, 1.000000000000000000, 0.000000000000000000 ) ) ;
#999 = CARTESIAN_POINT ( 'NONE',  ( -42.82802356641964536, 245.9948905601784759, -14.14213562373094746 ) ) ;
#1000 = EDGE_CURVE ( 'NONE', #12300, #2829, #19044, .T. ) ;
#1001 = CARTESIAN_POINT ( 'NONE',  ( -40.53162694259545162, 452.6198905683720568, -11.84573899990672707 ) ) ;
#1002 = VERTEX_POINT ( 'NONE', #8832 ) ;
#1003 = CARTESIAN_POINT ( 'NONE',  ( -36.33955658999051508, 445.3698905601785327, -18.47759065022572855 ) ) ;
#1004 = ORIENTED_EDGE ( 'NONE', *, *, #18546, .F. ) ;
#1005 = DIRECTION ( 'NONE',  ( -1.000000000000000000, 0.000000000000000000, 0.000000000000000000 ) ) ;
#1006 = ORIENTED_EDGE ( 'NONE', *, *, #6483, .F. ) ;
#1007 = ORIENTED_EDGE ( 'NONE', *, *, #9742, .T. ) ;
#1008 = DIRECTION ( 'NONE',  ( -1.000000000000000000, 0.000000000000000000, 0.000000000000000000 ) ) ;
#1009 = CARTESIAN_POINT ( 'NONE',  ( -48.68588794268870146, 317.2448905601784759, 0.000000000000000000 ) ) ;
#1010 = CARTESIAN_POINT ( 'NONE',  ( -14.48388495494900141, 371.3073905683721136, -9.489475012073734561 ) ) ;
#1011 = CARTESIAN_POINT ( 'NONE',  ( -1.084202172485504434E-15, -5.948846446048903225, 2.696295709017763720 ) ) ;
#1012 = CARTESIAN_POINT ( 'NONE',  ( -45.64106924314020119, 521.0573905765656946, -11.32908994701042715 ) ) ;
#1013 = CARTESIAN_POINT ( 'NONE',  ( -45.43829269268871940, 413.8698905683720568, 0.000000000000000000 ) ) ;
#1014 = CARTESIAN_POINT ( 'NONE',  ( -28.68588794268869790, 237.8698905683720568, 16.75240474999999307 ) ) ;
#1015 = CARTESIAN_POINT ( 'NONE',  ( -35.09675569278795138, 401.9948905683720568, -15.47720386886985544 ) ) ;
#1016 = ITEM_DEFINED_TRANSFORMATION ( 'NONE', 'NONE', #19366,  #12794 ) ;
#1017 = AXIS2_PLACEMENT_3D ( 'NONE', #12084, #13620, #8731 ) ;
#1018 = CARTESIAN_POINT ( 'NONE',  ( -48.68588794268870856, 342.3073905765656946, 3.978247347593168115 ) ) ;
#1019 = DIRECTION ( 'NONE',  ( 1.000000000000000000, 0.000000000000000000, 0.000000000000000000 ) ) ;
#1020 = CARTESIAN_POINT ( 'NONE',  ( -44.16309181155856578, 313.2448905683720000, -6.410867750099231266 ) ) ;
#1021 = CARTESIAN_POINT ( 'NONE',  ( -25.35362745456400191, 452.5573905683720568, -16.75240474999999307 ) ) ;
#1022 = CARTESIAN_POINT ( 'NONE',  ( -18.68588794268873698, 323.8848358243226357, -40.00000000000000000 ) ) ;
#1023 = LINE ( 'NONE', #14216, #41 ) ;
#1024 = DIRECTION ( 'NONE',  ( 1.000000000000000000, 0.000000000000000000, -0.000000000000000000 ) ) ;
#1025 = CARTESIAN_POINT ( 'NONE',  ( -42.88789093042843348, 366.3073905683720000, 9.489475012073736337 ) ) ;
#1026 = CARTESIAN_POINT ( 'NONE',  ( -44.16309181155857999, 494.4948905683720568, 6.410867750099241924 ) ) ;
#1027 = CARTESIAN_POINT ( 'NONE',  ( -36.33955658999052929, 515.3698905601784190, -18.47759065022572855 ) ) ;
#1028 = CARTESIAN_POINT ( 'NONE',  ( -32.01814843081344009, 321.6823905683720568, -16.75240474999999307 ) ) ;
#1029 = AXIS2_PLACEMENT_3D ( 'NONE', #12383, #12816, #15857 ) ;
#1030 = ORIENTED_EDGE ( 'NONE', *, *, #13546, .T. ) ;
#1031 = CARTESIAN_POINT ( 'NONE',  ( -16.84014894278200458, 497.6198905683720000, 11.84573899990672530 ) ) ;
#1032 = EDGE_LOOP ( 'NONE', ( #18693, #12072, #7439, #4372, #20196, #8855, #4075 ) ) ;
#1033 = CARTESIAN_POINT ( 'NONE',  ( 115.7989814974898337, 142.5259582928263455, 20.00000000000000355 ) ) ;
#1034 = CARTESIAN_POINT ( 'NONE',  ( -35.09675569278795138, 433.4948905683720568, -15.47720386886985544 ) ) ;
#1035 = CARTESIAN_POINT ( 'NONE',  ( 0.000000000000000000, 0.000000000000000000, 0.000000000000000000 ) ) ;
#1036 = DIRECTION ( 'NONE',  ( -1.000000000000000000, 0.000000000000000000, 0.000000000000000000 ) ) ;
#1037 = CARTESIAN_POINT ( 'NONE',  ( -40.53162694259545162, 465.1198905683720568, 11.84573899990672885 ) ) ;
#1038 = ORIENTED_EDGE ( 'NONE', *, *, #21391, .T. ) ;
#1039 = CARTESIAN_POINT ( 'NONE',  ( -25.35362745456400191, 461.0573905683720568, -16.75240474999999307 ) ) ;
#1040 = CARTESIAN_POINT ( 'NONE',  ( 72.94945500224395118, 285.0140030772282103, -20.00000000000000355 ) ) ;
#1041 = EDGE_CURVE ( 'NONE', #14194, #126, #311, .T. ) ;
#1042 = CARTESIAN_POINT ( 'NONE',  ( -32.66413529028188378, 399.8073905765656377, -19.99999999999999289 ) ) ;
#1043 = CARTESIAN_POINT ( 'NONE',  ( -8.685887942688706786, 226.9948905765656377, -2.449293598294705724E-15 ) ) ;
#1044 = DIRECTION ( 'NONE',  ( 0.000000000000000000, 0.000000000000000000, 1.000000000000000000 ) ) ;
#1045 = CARTESIAN_POINT ( 'NONE',  ( -31.26501780185373391, 205.1437886375728965, 0.000000000000000000 ) ) ;
#1046 = PLANE ( 'NONE',  #18730 ) ;
#1047 = ADVANCED_FACE ( 'NONE', ( #431 ), #16968, .F. ) ;
#1048 = EDGE_CURVE ( 'NONE', #11244, #13873, #10557, .T. ) ;
#1049 = CIRCLE ( 'NONE', #11375, 210.7252770684331438 ) ;
#1050 = ADVANCED_FACE ( 'NONE', ( #20627 ), #13825, .F. ) ;
#1051 = CARTESIAN_POINT ( 'NONE',  ( 51.93385628276429600, 30.52886280891152282, 94.99999999999994316 ) ) ;
#1052 = CARTESIAN_POINT ( 'NONE',  ( -28.68588794268874054, 588.2448905601785327, 0.000000000000000000 ) ) ;
#1053 = CARTESIAN_POINT ( 'NONE',  ( -46.31968306282883674, 160.1716627696692683, 33.59072564020503648 ) ) ;
#1054 = CARTESIAN_POINT ( 'NONE',  ( -32.66413529028186247, 245.0573905601785327, -19.99999999999999289 ) ) ;
#1055 = CARTESIAN_POINT ( 'NONE',  ( 78.68120802659203150, 149.7457237375499517, 40.00000000000000000 ) ) ;
#1056 = CARTESIAN_POINT ( 'NONE',  ( -35.09675569278795848, 427.2448905683720568, 15.47720386886985366 ) ) ;
#1057 = CARTESIAN_POINT ( 'NONE',  ( -40.53162694259542320, 246.6198905683720284, 11.84573899990672885 ) ) ;
#1058 = ADVANCED_FACE ( 'NONE', ( #20418 ), #5694, .T. ) ;
#1059 = ORIENTED_EDGE ( 'NONE', *, *, #16308, .T. ) ;
#1060 = ORIENTED_EDGE ( 'NONE', *, *, #18546, .T. ) ;
#1061 = PLANE ( 'NONE',  #2719 ) ;
#1062 = EDGE_LOOP ( 'NONE', ( #17844, #2192, #17637, #9146 ) ) ;
#1063 = CARTESIAN_POINT ( 'NONE',  ( -35.09675569278795848, 473.4948905683720000, -15.47720386886985544 ) ) ;
#1064 = VERTEX_POINT ( 'NONE', #7638 ) ;
#1065 = CARTESIAN_POINT ( 'NONE',  ( -22.27502019258947286, 240.7448905683720000, -15.47720386886985544 ) ) ;
#1066 = ORIENTED_EDGE ( 'NONE', *, *, #6841, .F. ) ;
#1067 =( BOUNDED_CURVE ( )  B_SPLINE_CURVE ( 2, ( #3378, #11261, #14956, #3054, #6603, #14530, #6390, #21225, #9531, #19491, #6716, #11478, #14853, #9957, #11588, #16149, #21114 ),
 .UNSPECIFIED., .F., .T. ) 
 B_SPLINE_CURVE_WITH_KNOTS ( ( 3, 2, 2, 2, 2, 2, 2, 2, 3 ),
 ( 0.7812500000000001110, 0.7832031250000001110, 0.7851562500000001110, 0.7871093750000001110, 0.7890625000000002220, 0.7910156250000002220, 0.7929687500000002220, 0.7949218750000002220, 0.7968750000000002220 ),
 .UNSPECIFIED. ) 
 CURVE ( )  GEOMETRIC_REPRESENTATION_ITEM ( )  RATIONAL_B_SPLINE_CURVE ( ( 0.9999999999999988898, 0.9807852804032315408, 1.000000000000000000, 0.9807852804032304306, 1.000000000000000000, 0.9807852804032304306, 1.000000000000000000, 0.9807852804032304306, 1.000000000000000000, 0.9807852804032304306, 1.000000000000000000, 0.9807852804032304306, 1.000000000000000000, 0.9807852804032304306, 1.000000000000000000, 0.9807852804032282101, 1.000000000000002220 ) ) 
 REPRESENTATION_ITEM ( '' )  );
#1068 = CARTESIAN_POINT ( 'NONE',  ( -13.20868407381887799, 518.2448905683720568, 6.410867750099229490 ) ) ;
#1069 = PLANE ( 'NONE',  #18679 ) ;
#1070 = CARTESIAN_POINT ( 'NONE',  ( -42.82802356641967378, 460.7448905765655809, -14.14213562373094746 ) ) ;
#1071 = CARTESIAN_POINT ( 'NONE',  ( 0.05533025579362307877, -6.264553569211845918, 2.149474931388140941 ) ) ;
#1072 = CARTESIAN_POINT ( 'NONE',  ( -14.54375231895775755, 285.7448905765655809, 14.14213562373094568 ) ) ;
#1073 = CARTESIAN_POINT ( 'NONE',  ( -40.01497788969915348, 455.6823905601785896, -16.95518130045146421 ) ) ;
#1074 = CARTESIAN_POINT ( 'NONE',  ( 5.700000000000000178, 0.000000000000000000, -4.400000000000000355 ) ) ;
#1075 = LINE ( 'NONE', #12307, #15304 ) ;
#1076 = CARTESIAN_POINT ( 'NONE',  ( -22.27502019258946220, 236.9948905683720284, 15.47720386886985189 ) ) ;
#1077 = CARTESIAN_POINT ( 'NONE',  ( -35.09675569278795138, 347.2448905683720000, 15.47720386886985366 ) ) ;
#1078 = CARTESIAN_POINT ( 'NONE',  ( 35.96497763894178945, 230.5765313837437418, -40.00000000000000000 ) ) ;
#1079 = AXIS2_PLACEMENT_3D ( 'NONE', #13026, #13357, #3610 ) ;
#1080 = CARTESIAN_POINT ( 'NONE',  ( -17.35679799567828852, 360.6823905601785327, 16.95518130045146421 ) ) ;
#1081 = CARTESIAN_POINT ( 'NONE',  ( -19.19641293061497933, 311.9323905683720568, -14.20200298773971603 ) ) ;
#1082 = CIRCLE ( 'NONE', #2490, 4.000000000000003553 ) ;
#1083 = CARTESIAN_POINT ( 'NONE',  ( -28.68588794268871567, 376.3698905683720568, 16.75240474999999307 ) ) ;
#1084 = VECTOR ( 'NONE', #12802, 1000.000000000000000 ) ;
#1085 = DIRECTION ( 'NONE',  ( -0.000000000000000000, -0.000000000000000000, 1.000000000000000000 ) ) ;
#1086 = AXIS2_PLACEMENT_3D ( 'NONE', #13564, #20152, #9973 ) ;
#1087 = CARTESIAN_POINT ( 'NONE',  ( -47.16347859291445133, 396.6198905601784759, -7.653668647301793193 ) ) ;
#1088 = CARTESIAN_POINT ( 'NONE',  ( 20.60949999999999349, 0.000000000000000000, 0.000000000000000000 ) ) ;
#1089 = EDGE_LOOP ( 'NONE', ( #10164, #17428, #9305, #19905 ) ) ;
#1090 = VERTEX_POINT ( 'NONE', #17595 ) ;
#1091 = CARTESIAN_POINT ( 'NONE',  ( -13.20868407381887621, 499.7448905683720000, 6.410867750099229490 ) ) ;
#1092 = CARTESIAN_POINT ( 'NONE',  ( -42.82802356641965247, 293.2448905765655809, 14.14213562373094923 ) ) ;
#1093 = ORIENTED_EDGE ( 'NONE', *, *, #16695, .T. ) ;
#1094 = CARTESIAN_POINT ( 'NONE',  ( -13.20868407381885135, 299.7448905683720568, 6.410867750099229490 ) ) ;
#1095 = ORIENTED_EDGE ( 'NONE', *, *, #17426, .F. ) ;
#1096 = CARTESIAN_POINT ( 'NONE',  ( -45.43829269268871229, 333.8698905683720000, 0.000000000000000000 ) ) ;
#1097 = ADVANCED_FACE ( 'NONE', ( #10662 ), #9263, .T. ) ;
#1098 = CARTESIAN_POINT ( 'NONE',  ( -24.70764059509555111, 259.1823905765656377, -19.99999999999999289 ) ) ;
#1099 = CARTESIAN_POINT ( 'NONE',  ( -8.685887942688509611, 497.3073905765656377, -3.978247347592607230 ) ) ;
#1100 = CARTESIAN_POINT ( 'NONE',  ( -19.19641293061496867, 240.4323905683720000, -14.20200298773971603 ) ) ;
#1101 = CARTESIAN_POINT ( 'NONE',  ( -13.20868407381886556, 400.9948905683720568, -6.410867750099233042 ) ) ;
#1102 = CARTESIAN_POINT ( 'NONE',  ( -24.70764059509555466, 334.4323905601785327, -19.99999999999999289 ) ) ;
#1103 = CYLINDRICAL_SURFACE ( 'NONE', #12822, 19.99999999999999645 ) ;
#1104 = EDGE_CURVE ( 'NONE', #13157, #1912, #14909, .T. ) ;
#1105 = CARTESIAN_POINT ( 'NONE',  ( -42.82802356641968089, 510.7448905765656946, -14.14213562373094746 ) ) ;
#1106 = CARTESIAN_POINT ( 'NONE',  ( -25.35362745456399125, 436.6823905683720000, 16.75240474999998952 ) ) ;
#1107 = VERTEX_POINT ( 'NONE', #10773 ) ;
#1108 = CARTESIAN_POINT ( 'NONE',  ( -21.03221929538691981, 440.3698905601784759, 18.47759065022572500 ) ) ;
#1109 = ORIENTED_EDGE ( 'NONE', *, *, #1652, .F. ) ;
#1110 = ORIENTED_EDGE ( 'NONE', *, *, #12732, .T. ) ;
#1111 = ORIENTED_EDGE ( 'NONE', *, *, #2578, .T. ) ;
#1112 = CARTESIAN_POINT ( 'NONE',  ( -8.938426032941704028E-16, 600.7448905601785327, 7.500000000000000000 ) ) ;
#1113 = AXIS2_PLACEMENT_3D ( 'NONE', #20332, #2170, #13424 ) ;
#1114 = CARTESIAN_POINT ( 'NONE',  ( -17.35679799567828852, 330.6823905601785327, 16.95518130045146421 ) ) ;
#1115 = CARTESIAN_POINT ( 'NONE',  ( -22.27502019258947641, 358.4948905683720000, 15.47720386886985189 ) ) ;
#1116 = CARTESIAN_POINT ( 'NONE',  ( 3.458603197740078627, 213.9102039777116602, -33.59072564020503648 ) ) ;
#1117 = CARTESIAN_POINT ( 'NONE',  ( -36.33955658999052218, 500.1198905765655809, -18.47759065022572855 ) ) ;
#1118 = CARTESIAN_POINT ( 'NONE',  ( -45.43829269268870519, 384.1823905683720000, 3.332260488124734632 ) ) ;
#1119 = CARTESIAN_POINT ( 'NONE',  ( -35.09675569278793006, 243.4948905683720284, -15.47720386886985544 ) ) ;
#1120 = CARTESIAN_POINT ( 'NONE',  ( -28.68588794268871922, 401.3698905683720000, -16.75240474999999307 ) ) ;
#1121 = EDGE_CURVE ( 'NONE', #8313, #3421, #9046, .T. ) ;
#1122 = CARTESIAN_POINT ( 'NONE',  ( -24.70764059509554755, 324.8073905765656946, 19.99999999999998934 ) ) ;
#1123 = CARTESIAN_POINT ( 'NONE',  ( 146.3141120573112630, 575.7448905601785327, 0.000000000000000000 ) ) ;
#1124 = CARTESIAN_POINT ( 'NONE',  ( -28.68588794268870856, 301.3698905683720568, -16.75240474999999307 ) ) ;
#1125 = CARTESIAN_POINT ( 'NONE',  ( -11.93348319268873148, 450.6823905683721136, -3.332260488124732856 ) ) ;
#1126 = LINE ( 'NONE', #9431, #4731 ) ;
#1127 = CARTESIAN_POINT ( 'NONE',  ( -49.57497958038185715, 160.1716627696692683, 60.00000000000000000 ) ) ;
#1128 = DIRECTION ( 'NONE',  ( -0.9365583756827543516, 0.000000000000000000, -0.3505116388060184329 ) ) ;
#1129 = VECTOR ( 'NONE', #91, 1000.000000000000000 ) ;
#1130 = CARTESIAN_POINT ( 'NONE',  ( -38.17536295476245556, 363.8073905683720568, -14.20200298773971426 ) ) ;
#1131 = CARTESIAN_POINT ( 'NONE',  ( -38.17536295476247687, 512.3073905683719431, -14.20200298773971426 ) ) ;
#1132 = CARTESIAN_POINT ( 'NONE',  ( -21.03221929538692692, 500.3698905601785327, 18.47759065022572500 ) ) ;
#1133 = CARTESIAN_POINT ( 'NONE',  ( -38.17536295476244135, 315.4323905683720000, 14.20200298773971781 ) ) ;
#1134 = EDGE_CURVE ( 'NONE', #18572, #20528, #15669, .T. ) ;
#1135 = EDGE_LOOP ( 'NONE', ( #11011, #16877 ) ) ;
#1136 = LINE ( 'NONE', #6295, #19374 ) ;
#1137 = EDGE_LOOP ( 'NONE', ( #13123, #13935, #1985, #5078, #11029, #2986, #11526, #5417, #8051, #16113 ) ) ;
#1138 = DIRECTION ( 'NONE',  ( 0.000000000000000000, 0.000000000000000000, -1.000000000000000000 ) ) ;
#1139 = CARTESIAN_POINT ( 'NONE',  ( -42.88789093042844058, 424.4323905683720568, -9.489475012073734561 ) ) ;
#1140 = CARTESIAN_POINT ( 'NONE',  ( -24.70764059509553334, 234.8073905765656377, 19.99999999999998934 ) ) ;
#1141 = DIRECTION ( 'NONE',  ( 0.000000000000000000, 0.000000000000000000, 1.000000000000000000 ) ) ;
#1142 = CARTESIAN_POINT ( 'NONE',  ( -13.20868407381886911, 448.2448905683720000, 6.410867750099229490 ) ) ;
#1143 = EDGE_LOOP ( 'NONE', ( #7066, #7328 ) ) ;
#1144 = CARTESIAN_POINT ( 'NONE',  ( -28.68588794268872988, 461.3698905683720000, -16.75240474999999307 ) ) ;
#1145 = CARTESIAN_POINT ( 'NONE',  ( -28.68588794268874409, 600.7448905601785327, -20.00000000000000355 ) ) ;
#1146 = ADVANCED_FACE ( 'NONE', ( #17281 ), #1069, .T. ) ;
#1147 = CARTESIAN_POINT ( 'NONE',  ( -42.82802356641966668, 413.2448905765655809, 14.14213562373094923 ) ) ;
#1148 = DIRECTION ( 'NONE',  ( -1.000000000000000000, -0.000000000000000000, -0.000000000000000000 ) ) ;
#1149 = CARTESIAN_POINT ( 'NONE',  ( 0.000000000000000000, 56.85652257517428865, 0.000000000000000000 ) ) ;
#1150 = DIRECTION ( 'NONE',  ( 0.000000000000000000, 0.000000000000000000, 1.000000000000000000 ) ) ;
#1151 = FACE_OUTER_BOUND ( 'NONE', #4117, .T. ) ;
#1152 = CARTESIAN_POINT ( 'NONE',  ( 60.03793209889851568, 10.52886280891152104, 131.1729372809869005 ) ) ;
#1153 = FACE_OUTER_BOUND ( 'NONE', #10681, .T. ) ;
#1154 = CARTESIAN_POINT ( 'NONE',  ( -45.11206863185022087, 223.9102039777116033, 6.767993150222416432 ) ) ;
#1155 = VECTOR ( 'NONE', #14617, 1000.000000000000114 ) ;
#1156 = CARTESIAN_POINT ( 'NONE',  ( -32.66413529028186247, 239.4323905601785043, 19.99999999999999289 ) ) ;
#1157 = CYLINDRICAL_SURFACE ( 'NONE', #9190, 19.99999999999999645 ) ;
#1158 = CARTESIAN_POINT ( 'NONE',  ( -13.20868407381886733, 420.9948905683720000, -6.410867750099233042 ) ) ;
#1159 = CARTESIAN_POINT ( 'NONE',  ( -48.68588794268854514, 386.9323905601785327, -3.978247347593583783 ) ) ;
#1160 = CARTESIAN_POINT ( 'NONE',  ( -13.20868407381884602, 249.7448905683720000, 6.410867750099229490 ) ) ;
#1161 = VERTEX_POINT ( 'NONE', #5802 ) ;
#1162 = VERTEX_POINT ( 'NONE', #13940 ) ;
#1163 = CARTESIAN_POINT ( 'NONE',  ( -13.20868407381887444, 470.9948905683720000, -6.410867750099233042 ) ) ;
#1164 = CARTESIAN_POINT ( 'NONE',  ( -8.685887942688708563, 236.9948905765656377, -2.449293598294705724E-15 ) ) ;
#1165 = VERTEX_POINT ( 'NONE', #17487 ) ;
#1166 = CARTESIAN_POINT ( 'NONE',  ( -17.35679799567830983, 525.4323905765656946, 16.95518130045146421 ) ) ;
#1167 = CARTESIAN_POINT ( 'NONE',  ( -16.84014894278197616, 250.1198905683720284, -11.84573899990672707 ) ) ;
#1168 = VECTOR ( 'NONE', #12818, 999.9999999999998863 ) ;
#1169 = ORIENTED_EDGE ( 'NONE', *, *, #3622, .T. ) ;
#1170 = CARTESIAN_POINT ( 'NONE',  ( -11.93348319268874214, 528.8698905683719431, -2.051577885510841163E-15 ) ) ;
#1171 = DIRECTION ( 'NONE',  ( 0.000000000000000000, 0.000000000000000000, 1.000000000000000000 ) ) ;
#1172 = CARTESIAN_POINT ( 'NONE',  ( -8.685887942688733432, 456.9948905765656377, -2.449293598294705724E-15 ) ) ;
#1173 = DIRECTION ( 'NONE',  ( 0.000000000000000000, 1.000000000000000000, -0.000000000000000000 ) ) ;
#1174 = DIRECTION ( 'NONE',  ( -1.000000000000000000, 0.000000000000000000, 0.000000000000000000 ) ) ;
#1175 = CARTESIAN_POINT ( 'NONE',  ( 30.42502041961813575, 271.1055109169419097, -40.00000000000000000 ) ) ;
#1176 = EDGE_CURVE ( 'NONE', #7385, #13157, #2466, .T. ) ;
#1177 = CARTESIAN_POINT ( 'NONE',  ( -19.19641293061496157, 228.8073905683720284, 14.20200298773971426 ) ) ;
#1178 = ADVANCED_FACE ( 'NONE', ( #9151 ), #8299, .T. ) ;
#1179 = CARTESIAN_POINT ( 'NONE',  ( 5.074999999999999289, 3.752776749732560368, -6.499999999999999112 ) ) ;
#1180 = CARTESIAN_POINT ( 'NONE',  ( -40.53162694259542320, 225.1198905683720000, 11.84573899990672885 ) ) ;
#1181 = CARTESIAN_POINT ( 'NONE',  ( -32.01814843081344009, 317.5573905683720568, 16.75240474999999307 ) ) ;
#1182 = VECTOR ( 'NONE', #7811, 1000.000000000000000 ) ;
#1183 = CARTESIAN_POINT ( 'NONE',  ( -41.83569717483972994, 303.6587712403113528, 25.00000000000000000 ) ) ;
#1184 = CARTESIAN_POINT ( 'NONE',  ( -6.276925316985670911, 585.7448905601785327, -44.69718552705352721 ) ) ;
#1185 = CONICAL_SURFACE ( 'NONE', #17068, 6.500000000000000000, 1.047197551196600296 ) ;
#1186 = VECTOR ( 'NONE', #651, 1000.000000000000000 ) ;
#1187 = CARTESIAN_POINT ( 'NONE',  ( -40.53162694259543031, 304.1198905683720000, -11.84573899990672707 ) ) ;
#1188 = CARTESIAN_POINT ( 'NONE',  ( -25.35362745456399480, 381.0573905683719431, -16.75240474999999307 ) ) ;
#1189 = CARTESIAN_POINT ( 'NONE',  ( -44.16309181155858710, 525.9948905683720568, 6.410867750099241924 ) ) ;
#1190 = CARTESIAN_POINT ( 'NONE',  ( -21.03221929538692692, 394.1198905601784759, -18.47759065022572855 ) ) ;
#1191 = CARTESIAN_POINT ( 'NONE',  ( -48.68588794268860198, 231.6823905765656377, -3.978247347593371508 ) ) ;
#1192 = VERTEX_POINT ( 'NONE', #18783 ) ;
#1193 = ORIENTED_EDGE ( 'NONE', *, *, #173, .T. ) ;
#1194 = CARTESIAN_POINT ( 'NONE',  ( -38.17536295476246977, 493.8073905683720000, -14.20200298773971426 ) ) ;
#1195 = CARTESIAN_POINT ( 'NONE',  ( -17.35679799567828141, 295.4323905765656377, 16.95518130045146421 ) ) ;
#1196 = VERTEX_POINT ( 'NONE', #3967 ) ;
#1197 = CARTESIAN_POINT ( 'NONE',  ( -42.88789093042842637, 294.4323905683720000, -9.489475012073734561 ) ) ;
#1198 = CARTESIAN_POINT ( 'NONE',  ( -13.20868407381885667, 329.4948905683720568, -6.410867750099233042 ) ) ;
#1199 = VECTOR ( 'NONE', #3391, 1000.000000000000000 ) ;
#1200 = CARTESIAN_POINT ( 'NONE',  ( -28.68588794268870146, 264.4948905765656377, 19.99999999999999289 ) ) ;
#1201 = CARTESIAN_POINT ( 'NONE',  ( -48.68588794268872277, 477.2448905601784759, 0.000000000000000000 ) ) ;
#1202 = DIRECTION ( 'NONE',  ( -1.191790137725560488E-16, 1.000000000000000000, -0.000000000000000000 ) ) ;
#1203 = CARTESIAN_POINT ( 'NONE',  ( -22.27502019258947996, 388.4948905683720000, 15.47720386886985189 ) ) ;
#1204 = CARTESIAN_POINT ( 'NONE',  ( -21.03221929538691981, 334.1198905601784759, -18.47759065022572855 ) ) ;
#1205 = LINE ( 'NONE', #17735, #6578 ) ;
#1206 = CARTESIAN_POINT ( 'NONE',  ( -18.68588794268873698, 323.8848358243226357, 20.00000000000000355 ) ) ;
#1207 = CARTESIAN_POINT ( 'NONE',  ( -28.68588794268872633, 441.3698905683720000, -16.75240474999999307 ) ) ;
#1208 = CYLINDRICAL_SURFACE ( 'NONE', #2725, 19.99999999999999645 ) ;
#1209 = ORIENTED_EDGE ( 'NONE', *, *, #18529, .T. ) ;
#1210 = CARTESIAN_POINT ( 'NONE',  ( -17.35679799567830273, 440.6823905601785327, 16.95518130045146421 ) ) ;
#1211 = ORIENTED_EDGE ( 'NONE', *, *, #11510, .F. ) ;
#1212 = ORIENTED_EDGE ( 'NONE', *, *, #6430, .T. ) ;
#1213 = VERTEX_POINT ( 'NONE', #2359 ) ;
#1214 = DIRECTION ( 'NONE',  ( 0.000000000000000000, 1.000000000000000000, 0.000000000000000000 ) ) ;
#1215 = CARTESIAN_POINT ( 'NONE',  ( -48.68588794268870146, 327.5573905601784759, 3.978247347593168115 ) ) ;
#1216 = CARTESIAN_POINT ( 'NONE',  ( -32.66413529028186957, 379.8073905765656377, -19.99999999999999289 ) ) ;
#1217 = CARTESIAN_POINT ( 'NONE',  ( -13.20868407381886023, 360.9948905683720568, -6.410867750099233042 ) ) ;
#1218 = CARTESIAN_POINT ( 'NONE',  ( 51.50493485826542184, 141.8799693780962912, 20.00000000000000355 ) ) ;
#1219 = CARTESIAN_POINT ( 'NONE',  ( -42.82802356641968089, 513.2448905765656946, 14.14213562373094923 ) ) ;
#1220 = CARTESIAN_POINT ( 'NONE',  ( -45.43829269268871229, 393.5573905683720568, -3.332260488124726194 ) ) ;
#1221 = CARTESIAN_POINT ( 'NONE',  ( -40.53162694259542320, 226.6198905683720000, 11.84573899990672885 ) ) ;
#1222 = CARTESIAN_POINT ( 'NONE',  ( -38.17536295476246266, 402.3073905683720000, -14.20200298773971426 ) ) ;
#1223 = CARTESIAN_POINT ( 'NONE',  ( -45.64106924314018698, 332.9323905765655809, 11.32908994701042715 ) ) ;
#1224 = CARTESIAN_POINT ( 'NONE',  ( -48.68588794268870146, 326.9323905601784759, -3.978247347593157901 ) ) ;
#1225 = CARTESIAN_POINT ( 'NONE',  ( -40.53162694259543031, 302.6198905683720000, -11.84573899990672707 ) ) ;
#1226 = CARTESIAN_POINT ( 'NONE',  ( -25.35362745456399125, 458.1823905683720000, 16.75240474999998952 ) ) ;
#1227 = CARTESIAN_POINT ( 'NONE',  ( -45.64106924314020119, 512.9323905765656946, 11.32908994701042538 ) ) ;
#1228 = LINE ( 'NONE', #14432, #10712 ) ;
#1229 = DIRECTION ( 'NONE',  ( 0.008660258604321402487, -0.3791853047755957551, 0.9252802302887190855 ) ) ;
#1230 = CARTESIAN_POINT ( 'NONE',  ( -40.53162694259543741, 364.1198905683720000, -11.84573899990672707 ) ) ;
#1231 = CARTESIAN_POINT ( 'NONE',  ( -35.09675569278796559, 495.7448905683720000, 15.47720386886985366 ) ) ;
#1232 = CARTESIAN_POINT ( 'NONE',  ( -47.16347859291446554, 516.6198905601784190, -7.653668647301793193 ) ) ;
#1233 = CARTESIAN_POINT ( 'NONE',  ( -42.88789093042842637, 314.8073905683721136, 9.489475012073736337 ) ) ;
#1234 = EDGE_CURVE ( 'NONE', #182, #5454, #6020, .T. ) ;
#1235 = VERTEX_POINT ( 'NONE', #4077 ) ;
#1236 = CARTESIAN_POINT ( 'NONE',  ( -42.82802356641968089, 525.9948905601785327, -14.14213562373094746 ) ) ;
#1237 = ORIENTED_EDGE ( 'NONE', *, *, #20816, .F. ) ;
#1238 = CARTESIAN_POINT ( 'NONE',  ( 5.674999999999999822, 0.000000000000000000, 0.000000000000000000 ) ) ;
#1239 = CARTESIAN_POINT ( 'NONE',  ( -14.48388495494900674, 419.4323905683720000, 9.489475012073731008 ) ) ;
#1240 = CARTESIAN_POINT ( 'NONE',  ( -10.20829729246299067, 396.3698905765656377, 7.653668647301790529 ) ) ;
#1241 = CARTESIAN_POINT ( 'NONE',  ( -25.35362745456400191, 441.0573905683720000, -16.75240474999999307 ) ) ;
#1242 = ORIENTED_EDGE ( 'NONE', *, *, #14883, .T. ) ;
#1243 = CARTESIAN_POINT ( 'NONE',  ( -32.01814843081345430, 471.6823905683720568, -16.75240474999999307 ) ) ;
#1244 = FACE_OUTER_BOUND ( 'NONE', #10818, .T. ) ;
#1245 = CARTESIAN_POINT ( 'NONE',  ( -11.73070664223724968, 376.0573905765656377, 11.32908994701042005 ) ) ;
#1246 = CARTESIAN_POINT ( 'NONE',  ( -48.68588794268870146, 281.9948905765656377, 0.000000000000000000 ) ) ;
#1247 = LINE ( 'NONE', #10965, #4397 ) ;
#1248 = CARTESIAN_POINT ( 'NONE',  ( -11.73070664223726034, 437.9323905765655809, -11.32908994701042538 ) ) ;
#1249 = CARTESIAN_POINT ( 'NONE',  ( -36.33955658999050087, 253.8698905765656093, 18.47759065022572500 ) ) ;
#1250 = EDGE_CURVE ( 'NONE', #16993, #19049, #14045, .T. ) ;
#1251 = CARTESIAN_POINT ( 'NONE',  ( 18.20947592957839234, 600.7448905601785327, 168.5995991907681457 ) ) ;
#1252 = CARTESIAN_POINT ( 'NONE',  ( -44.73859291656508219, 223.9102039777117454, 8.083073056675337043 ) ) ;
#1253 = CARTESIAN_POINT ( 'NONE',  ( -19.19641293061498999, 431.9323905683719431, -14.20200298773971603 ) ) ;
#1254 = CARTESIAN_POINT ( 'NONE',  ( -8.685887942688712116, 266.9948905765656377, -2.449293598294705724E-15 ) ) ;
#1255 = CARTESIAN_POINT ( 'NONE',  ( -25.35362745456397704, 242.5573905683720000, -16.75240474999999307 ) ) ;
#1256 = EDGE_CURVE ( 'NONE', #17485, #13185, #15990, .T. ) ;
#1257 = ORIENTED_EDGE ( 'NONE', *, *, #3412, .F. ) ;
#1258 = ORIENTED_EDGE ( 'NONE', *, *, #20909, .F. ) ;
#1259 = DIRECTION ( 'NONE',  ( 0.000000000000000000, 0.000000000000000000, -1.000000000000000000 ) ) ;
#1260 = ORIENTED_EDGE ( 'NONE', *, *, #878, .F. ) ;
#1261 = CARTESIAN_POINT ( 'NONE',  ( -19.19641293061499354, 468.8073905683719431, 14.20200298773971426 ) ) ;
#1262 = CARTESIAN_POINT ( 'NONE',  ( -17.35679799567828496, 228.5573905765656093, -16.95518130045146421 ) ) ;
#1263 = ORIENTED_EDGE ( 'NONE', *, *, #8344, .F. ) ;
#1264 = CARTESIAN_POINT ( 'NONE',  ( -43.63240530816144513, 209.9813655751484589, 1.306613905557859834 ) ) ;
#1265 = CARTESIAN_POINT ( 'NONE',  ( -45.43829269268873361, 535.3698905683720568, 0.000000000000000000 ) ) ;
#1266 = ORIENTED_EDGE ( 'NONE', *, *, #20112, .F. ) ;
#1267 = CARTESIAN_POINT ( 'NONE',  ( -13.20868407381887977, 528.2448905683720568, 6.410867750099229490 ) ) ;
#1268 = CARTESIAN_POINT ( 'NONE',  ( 10.41669750159067220, 172.9933428177121471, -50.00000000000000000 ) ) ;
#1269 = CARTESIAN_POINT ( 'NONE',  ( -28.68588794268872633, 449.4948905765655809, -19.99999999999999289 ) ) ;
#1270 = CYLINDRICAL_SURFACE ( 'NONE', #7188, 10.00000000000000355 ) ;
#1271 = DIRECTION ( 'NONE',  ( -0.000000000000000000, -0.000000000000000000, 1.000000000000000000 ) ) ;
#1272 = CARTESIAN_POINT ( 'NONE',  ( -8.685887942688617969, 237.3073905765656377, -3.978247347592952732 ) ) ;
#1273 = FACE_OUTER_BOUND ( 'NONE', #7868, .T. ) ;
#1274 = VECTOR ( 'NONE', #21065, 1000.000000000000000 ) ;
#1275 = LINE ( 'NONE', #14482, #18370 ) ;
#1276 = CARTESIAN_POINT ( 'NONE',  ( -25.35362745456396283, 226.6823905683720284, 16.75240474999998952 ) ) ;
#1277 = CARTESIAN_POINT ( 'NONE',  ( -14.48388495494899431, 311.3073905683720568, -9.489475012073736337 ) ) ;
#1278 = LINE ( 'NONE', #8067, #9545 ) ;
#1279 = CARTESIAN_POINT ( 'NONE',  ( 5.074999999999999289, 0.000000000000000000, 0.000000000000000000 ) ) ;
#1280 = CARTESIAN_POINT ( 'NONE',  ( -45.43829269268870519, 315.3698905683720568, 0.000000000000000000 ) ) ;
#1281 = AXIS2_PLACEMENT_3D ( 'NONE', #20836, #19309, #9358 ) ;
#1282 = CARTESIAN_POINT ( 'NONE',  ( -32.01814843081344719, 381.6823905683719431, -16.75240474999999307 ) ) ;
#1283 = CARTESIAN_POINT ( 'NONE',  ( -13.20868407381887799, 519.7448905683720568, 6.410867750099229490 ) ) ;
#1284 = EDGE_CURVE ( 'NONE', #6399, #21098, #51, .T. ) ;
#1285 = CARTESIAN_POINT ( 'NONE',  ( -45.64106924314018698, 368.1823905601785327, 11.32908994701042715 ) ) ;
#1286 = AXIS2_PLACEMENT_3D ( 'NONE', #15307, #20265, #17237 ) ;
#1287 = DIRECTION ( 'NONE',  ( 0.000000000000000000, 1.000000000000000000, -0.000000000000000000 ) ) ;
#1288 = ORIENTED_EDGE ( 'NONE', *, *, #5130, .F. ) ;
#1289 = CARTESIAN_POINT ( 'NONE',  ( -14.48388495494901029, 479.4323905683720568, 9.489475012073732785 ) ) ;
#1290 = CARTESIAN_POINT ( 'NONE',  ( -11.93348319268871194, 288.8698905683720568, -2.051577885510841163E-15 ) ) ;
#1291 = ORIENTED_EDGE ( 'NONE', *, *, #9300, .F. ) ;
#1292 = CARTESIAN_POINT ( 'NONE',  ( -16.84014894278197971, 289.1198905683720568, 11.84573899990672530 ) ) ;
#1293 = B_SPLINE_CURVE_WITH_KNOTS ( 'NONE', 3,
 ( #3535, #14801, #1710, #13493, #14908, #5044, #18239, #16636, #15017, #201, #11752, #16419, #10123, #16744, #1931, #6875, #20088, #18453, #3640, #10757 ),
 .UNSPECIFIED., .F., .F.,
 ( 4, 2, 2, 2, 2, 2, 2, 2, 2, 4 ),
 ( 1.977866534538390665E-18, 0.0009844208871748756206, 0.001968841774349749506, 0.002953262661524623609, 0.003937683548699496411, 0.004922104435874370514, 0.005906525323049244616, 0.006398735766636719398, 0.006890946210224195047, 0.007875367097399143743 ),
 .UNSPECIFIED. ) ;
#1294 = CARTESIAN_POINT ( 'NONE',  ( -16.84014894278198327, 327.6198905683720000, 11.84573899990672530 ) ) ;
#1295 = EDGE_CURVE ( 'NONE', #6060, #10209, #5912, .T. ) ;
#1296 = CIRCLE ( 'NONE', #17189, 40.00000000000000000 ) ;
#1297 = CARTESIAN_POINT ( 'NONE',  ( -11.73070664223723902, 267.9323905765656946, -11.32908994701042715 ) ) ;
#1298 = CARTESIAN_POINT ( 'NONE',  ( -28.68588794268872988, 474.7448905601784759, -19.99999999999999289 ) ) ;
#1299 = CARTESIAN_POINT ( 'NONE',  ( -32.01814843081343298, 231.6823905683720284, -16.75240474999999307 ) ) ;
#1300 = B_SPLINE_CURVE_WITH_KNOTS ( 'NONE', 3,
 ( #11564, #18152, #4544, #3349, #1735, #3030, #2927, #6576, #14505, #8308, #6261, #13199, #9507, #9614, #16231, #12766, #7875, #6152, #21296, #12873 ),
 .UNSPECIFIED., .F., .F.,
 ( 4, 2, 2, 2, 2, 2, 2, 2, 2, 4 ),
 ( 2.332952144782239016E-18, 0.0009844208871748760543, 0.001968841774349749506, 0.002953262661524623609, 0.003937683548699497278, 0.004922104435874371381, 0.005906525323049245484, 0.006398735766636720265, 0.006890946210224195914, 0.007875367097399143743 ),
 .UNSPECIFIED. ) ;
#1301 = EDGE_CURVE ( 'NONE', #2614, #5342, #7256, .T. ) ;
#1302 = CARTESIAN_POINT ( 'NONE',  ( -38.17536295476244845, 376.9323905683719431, 14.20200298773971781 ) ) ;
#1303 = EDGE_CURVE ( 'NONE', #4099, #4231, #20951, .T. ) ;
#1304 = AXIS2_PLACEMENT_3D ( 'NONE', #13978, #5727, #14081 ) ;
#1305 = CYLINDRICAL_SURFACE ( 'NONE', #8884, 19.99999999999999645 ) ;
#1306 = CARTESIAN_POINT ( 'NONE',  ( -28.68588794268875120, 585.7448905601785327, 0.000000000000000000 ) ) ;
#1307 =( BOUNDED_CURVE ( )  B_SPLINE_CURVE ( 2, ( #6046, #5723, #19249, #17312, #9077, #14076, #20659, #5830, #12439, #8862, #4431, #12556, #4326, #11015, #10909, #11340, #9504 ),
 .UNSPECIFIED., .F., .T. ) 
 B_SPLINE_CURVE_WITH_KNOTS ( ( 3, 2, 2, 2, 2, 2, 2, 2, 3 ),
 ( 0.4375000000000002220, 0.4394531250000002220, 0.4414062500000002220, 0.4433593750000002220, 0.4453125000000002220, 0.4472656250000002220, 0.4492187500000002220, 0.4511718750000002220, 0.4531250000000002220 ),
 .UNSPECIFIED. ) 
 CURVE ( )  GEOMETRIC_REPRESENTATION_ITEM ( )  RATIONAL_B_SPLINE_CURVE ( ( 0.9999999999999977796, 0.9807852804032326510, 1.000000000000000000, 0.9807852804032304306, 1.000000000000000000, 0.9807852804032304306, 1.000000000000000000, 0.9807852804032304306, 1.000000000000000000, 0.9807852804032304306, 1.000000000000000000, 0.9807852804032304306, 1.000000000000000000, 0.9807852804032304306, 1.000000000000000000, 0.9807852804032282101, 1.000000000000002220 ) ) 
 REPRESENTATION_ITEM ( '' )  );
#1308 = CARTESIAN_POINT ( 'NONE',  ( 14.09825962131072785, 303.6587712403113528, 49.99999999999999289 ) ) ;
#1309 = CARTESIAN_POINT ( 'NONE',  ( -11.93348319268873148, 448.5573905683720000, 3.332260488124728415 ) ) ;
#1310 = CARTESIAN_POINT ( 'NONE',  ( 51.50493485826542184, 141.8799693780962912, 40.00000000000000000 ) ) ;
#1311 = EDGE_LOOP ( 'NONE', ( #5524, #18269, #18060, #3020, #1237, #19215 ) ) ;
#1312 = CARTESIAN_POINT ( 'NONE',  ( -45.64106924314019409, 436.3073905601784759, -11.32908994701042715 ) ) ;
#1313 = ADVANCED_FACE ( 'NONE', ( #14577 ), #8057, .T. ) ;
#1314 = ORIENTED_EDGE ( 'NONE', *, *, #12746, .F. ) ;
#1315 = ORIENTED_EDGE ( 'NONE', *, *, #18124, .T. ) ;
#1316 = VERTEX_POINT ( 'NONE', #9580 ) ;
#1317 = CARTESIAN_POINT ( 'NONE',  ( -43.15102588740141698, 208.1950015687324651, -3.974285180378252402 ) ) ;
#1318 = CARTESIAN_POINT ( 'NONE',  ( -40.01497788969913216, 325.6823905601785327, -16.95518130045146421 ) ) ;
#1319 = CARTESIAN_POINT ( 'NONE',  ( -11.73070664223725679, 417.9323905765656377, -11.32908994701042538 ) ) ;
#1320 = CARTESIAN_POINT ( 'NONE',  ( -11.93348319268872260, 350.0573905683720000, 3.332260488124728859 ) ) ;
#1321 = CARTESIAN_POINT ( 'NONE',  ( -24.70764059509557953, 499.1823905765656377, -19.99999999999999289 ) ) ;
#1322 = CARTESIAN_POINT ( 'NONE',  ( -22.27502019258949062, 380.7448905683720000, -15.47720386886985544 ) ) ;
#1323 = CARTESIAN_POINT ( 'NONE',  ( -162.2727221670389781, 30.52886280891152282, 0.000000000000000000 ) ) ;
#1324 = CARTESIAN_POINT ( 'NONE',  ( -45.43829269268871229, 384.1823905683720568, 3.332260488124734632 ) ) ;
#1325 = CARTESIAN_POINT ( 'NONE',  ( -32.66413529028186957, 324.1823905765655809, 19.99999999999999289 ) ) ;
#1326 = CARTESIAN_POINT ( 'NONE',  ( -36.33955658999051508, 425.3698905601784759, -18.47759065022572855 ) ) ;
#1327 = CARTESIAN_POINT ( 'NONE',  ( -22.27502019258946575, 276.9948905683720000, 15.47720386886985189 ) ) ;
#1328 = CARTESIAN_POINT ( 'NONE',  ( -13.20868407381886733, 439.7448905683720000, 6.410867750099229490 ) ) ;
#1329 = DIRECTION ( 'NONE',  ( -1.191790137725560488E-16, 1.000000000000000000, -0.000000000000000000 ) ) ;
#1330 = CARTESIAN_POINT ( 'NONE',  ( -40.01497788969913216, 368.8073905601785327, 16.95518130045146776 ) ) ;
#1331 = DIRECTION ( 'NONE',  ( 0.000000000000000000, 0.000000000000000000, -1.000000000000000000 ) ) ;
#1332 = CARTESIAN_POINT ( 'NONE',  ( -45.43829269268871229, 345.3698905683720568, 0.000000000000000000 ) ) ;
#1333 = CARTESIAN_POINT ( 'NONE',  ( -35.09675569278796559, 511.9948905683720000, -15.47720386886985544 ) ) ;
#1334 = CARTESIAN_POINT ( 'NONE',  ( -24.70764059509557953, 504.4323905601785327, -19.99999999999999289 ) ) ;
#1335 = CARTESIAN_POINT ( 'NONE',  ( -13.20868407381885667, 329.4948905683720568, -6.410867750099233042 ) ) ;
#1336 = EDGE_LOOP ( 'NONE', ( #2701, #4093, #17098, #4444 ) ) ;
#1337 = CARTESIAN_POINT ( 'NONE',  ( -45.64106924314016567, 258.1823905601784190, 11.32908994701042538 ) ) ;
#1338 = VERTEX_POINT ( 'NONE', #7945 ) ;
#1339 = LINE ( 'NONE', #4681, #4640 ) ;
#1340 = CIRCLE ( 'NONE', #13434, 5.000000000000004441 ) ;
#1341 = CARTESIAN_POINT ( 'NONE',  ( -35.09675569278795848, 427.2448905683720568, 15.47720386886985366 ) ) ;
#1342 = CARTESIAN_POINT ( 'NONE',  ( -36.33955658999050087, 233.8698905765656093, 18.47759065022572500 ) ) ;
#1343 =( LENGTH_UNIT ( ) NAMED_UNIT ( * ) SI_UNIT ( .MILLI., .METRE. ) );
#1344 = CARTESIAN_POINT ( 'NONE',  ( -44.16309181155857289, 434.4948905683720568, 6.410867750099241924 ) ) ;
#1345 = ORIENTED_EDGE ( 'NONE', *, *, #1971, .T. ) ;
#1346 = CARTESIAN_POINT ( 'NONE',  ( -40.53162694259545162, 452.6198905683720568, -11.84573899990672707 ) ) ;
#1347 = CARTESIAN_POINT ( 'NONE',  ( 0.000000000000000000, 390.7481941534130101, 0.000000000000000000 ) ) ;
#1348 = CARTESIAN_POINT ( 'NONE',  ( 88.28695088269886071, 152.5259582928263740, -20.00000000000000355 ) ) ;
#1349 = CARTESIAN_POINT ( 'NONE',  ( -11.73070664223725146, 377.9323905765656946, -11.32908994701042715 ) ) ;
#1350 = CARTESIAN_POINT ( 'NONE',  ( -28.68588794268874054, 573.2448905601785327, 0.000000000000000000 ) ) ;
#1351 = DIRECTION ( 'NONE',  ( 0.000000000000000000, 0.000000000000000000, 1.000000000000000000 ) ) ;
#1352 = CARTESIAN_POINT ( 'NONE',  ( -28.68588794268872277, 429.4948905765655809, -19.99999999999999289 ) ) ;
#1353 = CARTESIAN_POINT ( 'NONE',  ( -8.938426032941704028E-16, 600.7448905601785327, 7.500000000000000000 ) ) ;
#1354 = CARTESIAN_POINT ( 'NONE',  ( -38.17536295476246977, 516.9323905683720568, 14.20200298773971781 ) ) ;
#1355 = EDGE_CURVE ( 'NONE', #18698, #18459, #11098, .T. ) ;
#1356 = CARTESIAN_POINT ( 'NONE',  ( 91.21585410611801592, 56.85652257517428865, 94.99999999999994316 ) ) ;
#1357 = CARTESIAN_POINT ( 'NONE',  ( -10.20829729246297291, 252.8698905601785043, -7.653668647301794969 ) ) ;
#1358 = CIRCLE ( 'NONE', #2054, 6.500000000000000888 ) ;
#1359 = CARTESIAN_POINT ( 'NONE',  ( -19.19641293061498999, 421.9323905683720000, -14.20200298773971603 ) ) ;
#1360 = CARTESIAN_POINT ( 'NONE',  ( -14.54375231895775578, 265.7448905765656377, 14.14213562373094568 ) ) ;
#1361 = CARTESIAN_POINT ( 'NONE',  ( -28.68588794268869790, 247.8698905683720000, 16.75240474999999307 ) ) ;
#1362 = EDGE_LOOP ( 'NONE', ( #15988, #9440, #20923, #7596 ) ) ;
#1363 = EDGE_LOOP ( 'NONE', ( #16478, #925, #12624, #3143 ) ) ;
#1364 = DIRECTION ( 'NONE',  ( 0.000000000000000000, 0.000000000000000000, -1.000000000000000000 ) ) ;
#1365 = ORIENTED_EDGE ( 'NONE', *, *, #5370, .T. ) ;
#1366 = AXIS2_PLACEMENT_3D ( 'NONE', #21265, #13048, #3732 ) ;
#1367 = CARTESIAN_POINT ( 'NONE',  ( -44.16309181155858710, 464.7448905683720568, -6.410867750099231266 ) ) ;
#1368 = CARTESIAN_POINT ( 'NONE',  ( -18.67112375231569743, 218.6607918971888864, -17.31197557216455252 ) ) ;
#1369 = ADVANCED_FACE ( 'NONE', ( #4931 ), #11208, .T. ) ;
#1370 = ORIENTED_EDGE ( 'NONE', *, *, #11144, .T. ) ;
#1371 = CARTESIAN_POINT ( 'NONE',  ( -43.31915179403467420, 208.9097650327693430, 3.305147470758841077 ) ) ;
#1372 = CARTESIAN_POINT ( 'NONE',  ( -25.35362745456401257, 532.5573905683720568, -16.75240474999999307 ) ) ;
#1373 = ORIENTED_EDGE ( 'NONE', *, *, #878, .T. ) ;
#1374 = CARTESIAN_POINT ( 'NONE',  ( -45.43829269268873361, 523.8698905683720568, 0.000000000000000000 ) ) ;
#1375 = DIRECTION ( 'NONE',  ( -1.000000000000000000, 0.000000000000000000, -2.399110633850889130E-16 ) ) ;
#1376 = CARTESIAN_POINT ( 'NONE',  ( -40.01497788969915348, 450.4323905765656946, -16.95518130045146421 ) ) ;
#1377 = CARTESIAN_POINT ( 'NONE',  ( -24.70764059509554755, 350.0573905601785327, 19.99999999999998934 ) ) ;
#1378 = CARTESIAN_POINT ( 'NONE',  ( -11.93348319268871904, 348.8698905683720568, -2.051577885510841163E-15 ) ) ;
#1379 = CARTESIAN_POINT ( 'NONE',  ( 40.42502041961814996, 170.1716627696692683, -20.00000000000000355 ) ) ;
#1380 = DIRECTION ( 'NONE',  ( -1.191790137725560488E-16, 1.000000000000000000, -0.000000000000000000 ) ) ;
#1381 = CARTESIAN_POINT ( 'NONE',  ( -28.68588794268874054, 333.8848358243226357, 40.00000000000000000 ) ) ;
#1382 = EDGE_CURVE ( 'NONE', #14089, #19571, #18016, .T. ) ;
#1383 = CARTESIAN_POINT ( 'NONE',  ( -24.73359481245773495, 223.9102039777117454, 19.67196200432813313 ) ) ;
#1384 = CARTESIAN_POINT ( 'NONE',  ( -25.35362745456397704, 231.0573905683720568, -16.75240474999999307 ) ) ;
#1385 = CARTESIAN_POINT ( 'NONE',  ( -28.68588794268870501, 307.8698905683720000, 16.75240474999999307 ) ) ;
#1386 = CARTESIAN_POINT ( 'NONE',  ( -28.68588794268872633, 444.7448905601784759, -19.99999999999999289 ) ) ;
#1387 = CARTESIAN_POINT ( 'NONE',  ( 0.000000000000000000, 0.000000000000000000, 6.500000000000000000 ) ) ;
#1388 = CARTESIAN_POINT ( 'NONE',  ( -42.88789093042842637, 316.3073905683720568, 9.489475012073736337 ) ) ;
#1389 = CARTESIAN_POINT ( 'NONE',  ( -45.43829269268870519, 354.1823905683721136, 3.332260488124734632 ) ) ;
#1390 = CARTESIAN_POINT ( 'NONE',  ( -19.19641293061500420, 531.9323905683720568, -14.20200298773971603 ) ) ;
#1391 = CARTESIAN_POINT ( 'NONE',  ( -48.68588794268870856, 367.2448905601784759, 0.000000000000000000 ) ) ;
#1392 = EDGE_CURVE ( 'NONE', #1858, #4099, #16411, .T. ) ;
#1393 = LINE ( 'NONE', #6036, #14986 ) ;
#1394 = EDGE_LOOP ( 'NONE', ( #2018, #1886, #15579, #4337 ) ) ;
#1395 = CARTESIAN_POINT ( 'NONE',  ( -44.16309181155857999, 495.9948905683720568, 6.410867750099241924 ) ) ;
#1396 = DIRECTION ( 'NONE',  ( 0.000000000000000000, 1.000000000000000000, 0.000000000000000000 ) ) ;
#1397 = CARTESIAN_POINT ( 'NONE',  ( -35.09675569278794427, 275.7448905683720568, 15.47720386886985366 ) ) ;
#1398 = ORIENTED_EDGE ( 'NONE', *, *, #9876, .T. ) ;
#1399 = CIRCLE ( 'NONE', #13495, 21.20245194746113526 ) ;
#1400 = CARTESIAN_POINT ( 'NONE',  ( -22.27502019258947996, 292.2448905683720000, -15.47720386886985544 ) ) ;
#1401 = CARTESIAN_POINT ( 'NONE',  ( -22.27502019258947286, 326.9948905683720000, 15.47720386886985189 ) ) ;
#1402 = CARTESIAN_POINT ( 'NONE',  ( -42.88789093042841927, 264.4323905683720568, -9.489475012073734561 ) ) ;
#1403 = CARTESIAN_POINT ( 'NONE',  ( -48.68588794268870146, 272.3073905765656377, 3.978247347593168115 ) ) ;
#1404 = DIRECTION ( 'NONE',  ( 0.000000000000000000, 0.000000000000000000, -1.000000000000000000 ) ) ;
#1405 = CARTESIAN_POINT ( 'NONE',  ( -45.43829269268869808, 234.1823905683720284, 3.332260488124734632 ) ) ;
#1406 = CARTESIAN_POINT ( 'NONE',  ( -11.93348319268872260, 380.6823905683720568, -3.332260488124732856 ) ) ;
#1407 = CARTESIAN_POINT ( 'NONE',  ( -33.07955326574332133, 585.7448905601785327, 10.74819839862556492 ) ) ;
#1408 = CIRCLE ( 'NONE', #8309, 15.00000000000000000 ) ;
#1409 = CARTESIAN_POINT ( 'NONE',  ( -17.35679799567830628, 458.5573905765656946, -16.95518130045146421 ) ) ;
#1410 = VECTOR ( 'NONE', #483, 1000.000000000000000 ) ;
#1411 = CARTESIAN_POINT ( 'NONE',  ( 5.074999999999999289, 3.752776749732562589, 6.500000000000000000 ) ) ;
#1412 = CARTESIAN_POINT ( 'NONE',  ( -45.43829269268871229, 414.1823905683720000, 3.332260488124734632 ) ) ;
#1413 = CARTESIAN_POINT ( 'NONE',  ( -49.57497958038185715, 160.1716627696692683, -50.00000000000000000 ) ) ;
#1414 = EDGE_LOOP ( 'NONE', ( #2541, #10703, #17353, #15763, #10706 ) ) ;
#1415 = AXIS2_PLACEMENT_3D ( 'NONE', #17806, #14791, #21161 ) ;
#1416 = CARTESIAN_POINT ( 'NONE',  ( -48.68588794268871567, 417.5573905601784759, 3.978247347593168115 ) ) ;
#1417 = ORIENTED_EDGE ( 'NONE', *, *, #5038, .F. ) ;
#1418 = ORIENTED_EDGE ( 'NONE', *, *, #958, .F. ) ;
#1419 = CARTESIAN_POINT ( 'NONE',  ( -43.47609127650945737, 209.4774105891669933, -2.515022083182098189 ) ) ;
#1420 = CARTESIAN_POINT ( 'NONE',  ( -8.685887942688715668, 311.9323905601784759, 3.978247347593161010 ) ) ;
#1421 = DIRECTION ( 'NONE',  ( 0.000000000000000000, 0.000000000000000000, -1.000000000000000000 ) ) ;
#1422 = EDGE_CURVE ( 'NONE', #18669, #17480, #19322, .T. ) ;
#1423 = CARTESIAN_POINT ( 'NONE',  ( -19.19641293061497578, 338.8073905683720000, 14.20200298773971426 ) ) ;
#1424 = AXIS2_PLACEMENT_3D ( 'NONE', #21238, #11062, #9862 ) ;
#1425 = CIRCLE ( 'NONE', #2461, 200.0000000000000000 ) ;
#1426 = CARTESIAN_POINT ( 'NONE',  ( -48.68588794268872988, 511.9948905765656377, 0.000000000000000000 ) ) ;
#1427 = CARTESIAN_POINT ( 'NONE',  ( -38.17536295476244845, 375.4323905683720568, 14.20200298773971781 ) ) ;
#1428 = CARTESIAN_POINT ( 'NONE',  ( -11.93348319268870483, 230.3698905683720284, -2.051577885510841163E-15 ) ) ;
#1429 = CARTESIAN_POINT ( 'NONE',  ( -38.17536295476245556, 382.3073905683719431, -14.20200298773971426 ) ) ;
#1430 = CARTESIAN_POINT ( 'NONE',  ( -8.685887942688717445, 327.3073905765656377, -3.978247347593165895 ) ) ;
#1431 = DIRECTION ( 'NONE',  ( 0.000000000000000000, 1.000000000000000000, 0.000000000000000000 ) ) ;
#1432 = CARTESIAN_POINT ( 'NONE',  ( -32.01814843081344009, 281.6823905683720000, -16.75240474999999307 ) ) ;
#1433 = AXIS2_PLACEMENT_3D ( 'NONE', #11035, #7577, #6678 ) ;
#1434 =( BOUNDED_CURVE ( )  B_SPLINE_CURVE ( 2, ( #15145, #20106, #16867, #15037, #20211, #327, #221, #13407, #109, #2049, #11771, #18576, #3344, #5376, #8623, #7000, #19996 ),
 .UNSPECIFIED., .F., .T. ) 
 B_SPLINE_CURVE_WITH_KNOTS ( ( 3, 2, 2, 2, 2, 2, 2, 2, 3 ),
 ( 0.7031250000000002220, 0.7050781250000002220, 0.7070312500000002220, 0.7089843750000002220, 0.7109375000000002220, 0.7128906250000002220, 0.7148437500000002220, 0.7167968750000002220, 0.7187500000000002220 ),
 .UNSPECIFIED. ) 
 CURVE ( )  GEOMETRIC_REPRESENTATION_ITEM ( )  RATIONAL_B_SPLINE_CURVE ( ( 0.9999999999999977796, 0.9807852804032326510, 1.000000000000000000, 0.9807852804032304306, 1.000000000000000000, 0.9807852804032304306, 1.000000000000000000, 0.9807852804032304306, 1.000000000000000000, 0.9807852804032304306, 1.000000000000000000, 0.9807852804032304306, 1.000000000000000000, 0.9807852804032304306, 1.000000000000000000, 0.9807852804032282101, 1.000000000000002220 ) ) 
 REPRESENTATION_ITEM ( '' )  );
#1435 = CARTESIAN_POINT ( 'NONE',  ( -14.48388495494900496, 439.4323905683720000, 9.489475012073732785 ) ) ;
#1436 = ADVANCED_FACE ( 'NONE', ( #4509 ), #9895, .T. ) ;
#1437 = CARTESIAN_POINT ( 'NONE',  ( 14.09825962131072785, 230.5765313837437418, 25.00000000000000000 ) ) ;
#1438 = CARTESIAN_POINT ( 'NONE',  ( 0.1061556211655336340, 6.421950209808279020, 1.876855952934451732 ) ) ;
#1439 = DIRECTION ( 'NONE',  ( 0.8090169943749474513, 0.000000000000000000, 0.5877852522924730261 ) ) ;
#1440 = CARTESIAN_POINT ( 'NONE',  ( -38.17536295476245556, 353.8073905683720568, -14.20200298773971426 ) ) ;
#1441 = CARTESIAN_POINT ( 'NONE',  ( -44.16309181155858710, 503.2448905683719431, -6.410867750099231266 ) ) ;
#1442 = CIRCLE ( 'NONE', #11790, 28.29169339157297358 ) ;
#1443 = CARTESIAN_POINT ( 'NONE',  ( -45.64106924314020119, 478.1823905601784759, 11.32908994701042715 ) ) ;
#1444 = CARTESIAN_POINT ( 'NONE',  ( -11.93348319268871727, 318.5573905683720000, 3.332260488124728415 ) ) ;
#1445 = ORIENTED_EDGE ( 'NONE', *, *, #3274, .F. ) ;
#1446 = DIRECTION ( 'NONE',  ( -0.000000000000000000, 1.000000000000000000, -0.000000000000000000 ) ) ;
#1447 = VERTEX_POINT ( 'NONE', #1268 ) ;
#1448 = CARTESIAN_POINT ( 'NONE',  ( -33.07955326574333554, 600.7448905601785327, -10.74819839862556314 ) ) ;
#1449 = CARTESIAN_POINT ( 'NONE',  ( -11.93348319268872615, 410.3698905683720568, -2.051577885510841163E-15 ) ) ;
#1450 = CARTESIAN_POINT ( 'NONE',  ( -48.68588794268871567, 397.2448905601784759, 0.000000000000000000 ) ) ;
#1451 = LINE ( 'NONE', #11174, #16626 ) ;
#1452 = CARTESIAN_POINT ( 'NONE',  ( -40.53162694259545162, 452.6198905683720568, -11.84573899990672707 ) ) ;
#1453 = CARTESIAN_POINT ( 'NONE',  ( -28.68588794268872277, 446.3698905683720000, 16.75240474999999307 ) ) ;
#1454 = DIRECTION ( 'NONE',  ( 0.000000000000000000, 0.000000000000000000, 1.000000000000000000 ) ) ;
#1455 = CARTESIAN_POINT ( 'NONE',  ( -8.685887942688726326, 402.2448905601784759, -2.449293598294705724E-15 ) ) ;
#1456 = CARTESIAN_POINT ( 'NONE',  ( -36.33955658999051508, 390.1198905765656377, -18.47759065022572855 ) ) ;
#1457 = CARTESIAN_POINT ( 'NONE',  ( -28.68588794268873343, 47.23886018424757083, 49.60091809715359545 ) ) ;
#1458 = DIRECTION ( 'NONE',  ( 1.000000000000000000, 0.000000000000000000, 0.000000000000000000 ) ) ;
#1459 = CARTESIAN_POINT ( 'NONE',  ( -8.685887942688642838, 427.3073905765655809, -3.978247347592952732 ) ) ;
#1460 = CYLINDRICAL_SURFACE ( 'NONE', #1079, 19.99999999999999645 ) ;
#1461 = AXIS2_PLACEMENT_3D ( 'NONE', #2129, #11857, #15336 ) ;
#1462 = CARTESIAN_POINT ( 'NONE',  ( -42.88789093042844769, 494.4323905683720000, -9.489475012073736337 ) ) ;
#1463 = DIRECTION ( 'NONE',  ( 1.000000000000000000, 0.000000000000000000, -0.000000000000000000 ) ) ;
#1464 = LINE ( 'NONE', #6207, #13909 ) ;
#1465 = CARTESIAN_POINT ( 'NONE',  ( -24.70764059509555466, 420.0573905601784190, 19.99999999999998934 ) ) ;
#1466 = CARTESIAN_POINT ( 'NONE',  ( -45.43829269268871940, 405.3698905683720000, 0.000000000000000000 ) ) ;
#1467 = CARTESIAN_POINT ( 'NONE',  ( -8.685887942688546914, 382.5573905601784190, -3.978247347592740013 ) ) ;
#1468 = CARTESIAN_POINT ( 'NONE',  ( -13.20868407381884602, 239.7448905683720000, 6.410867750099229490 ) ) ;
#1469 = ORIENTED_EDGE ( 'NONE', *, *, #331, .T. ) ;
#1470 = CYLINDRICAL_SURFACE ( 'NONE', #4091, 5.000000000000004441 ) ;
#1471 = VERTEX_POINT ( 'NONE', #17701 ) ;
#1472 = CARTESIAN_POINT ( 'NONE',  ( -35.09675569278796559, 457.2448905683720568, 15.47720386886985366 ) ) ;
#1473 = CARTESIAN_POINT ( 'NONE',  ( -8.685887942688706786, 226.6823905765656377, 3.978247347593161010 ) ) ;
#1474 = ORIENTED_EDGE ( 'NONE', *, *, #8471, .T. ) ;
#1475 = CARTESIAN_POINT ( 'NONE',  ( -43.52342829599625418, 209.6345393943126396, 2.222589281884804979 ) ) ;
#1476 = CARTESIAN_POINT ( 'NONE',  ( -32.01814843081343298, 221.6823905683720000, -16.75240474999999307 ) ) ;
#1477 = ORIENTED_EDGE ( 'NONE', *, *, #4146, .F. ) ;
#1478 = EDGE_CURVE ( 'NONE', #8423, #10551, #19637, .T. ) ;
#1479 = CARTESIAN_POINT ( 'NONE',  ( -13.20868407381887799, 509.4948905683720568, -6.410867750099233042 ) ) ;
#1480 = DIRECTION ( 'NONE',  ( 1.000000000000000000, 0.000000000000000000, -0.000000000000000000 ) ) ;
#1481 = CARTESIAN_POINT ( 'NONE',  ( -36.33955658999051508, 440.1198905765656377, -18.47759065022572855 ) ) ;
#1482 = CARTESIAN_POINT ( 'NONE',  ( -48.68588794268843145, 361.6823905765655240, -3.978247347593797389 ) ) ;
#1483 = EDGE_CURVE ( 'NONE', #1002, #15603, #7743, .T. ) ;
#1484 = DIRECTION ( 'NONE',  ( 0.000000000000000000, 0.000000000000000000, -1.000000000000000000 ) ) ;
#1485 = DIRECTION ( 'NONE',  ( -1.232945044042657126E-32, 9.855701800883825964E-17, 1.000000000000000000 ) ) ;
#1486 = CARTESIAN_POINT ( 'NONE',  ( -48.68588794268870146, 287.2448905601784759, 0.000000000000000000 ) ) ;
#1487 = AXIS2_PLACEMENT_3D ( 'NONE', #3001, #1485, #3107 ) ;
#1488 = CARTESIAN_POINT ( 'NONE',  ( -32.77073113723689346, 223.9102039777117454, 19.64486615283885840 ) ) ;
#1489 = CARTESIAN_POINT ( 'NONE',  ( -45.43829269268869808, 233.8698905683720284, 0.000000000000000000 ) ) ;
#1490 = B_SPLINE_CURVE_WITH_KNOTS ( 'NONE', 3,
 ( #21379, #6548, #11535, #12736, #9378, #9691 ),
 .UNSPECIFIED., .F., .F.,
 ( 4, 2, 4 ),
 ( 2.380733003139562229E-07, 0.001898835937927372897, 0.003797433802554431564 ),
 .UNSPECIFIED. ) ;
#1491 = CARTESIAN_POINT ( 'NONE',  ( -19.19641293061498288, 321.9323905683720000, -14.20200298773971603 ) ) ;
#1492 = DIRECTION ( 'NONE',  ( -1.000000000000000000, -0.000000000000000000, -0.000000000000000000 ) ) ;
#1493 = CARTESIAN_POINT ( 'NONE',  ( -8.685887942688710339, 261.9323905601784759, 3.978247347593161010 ) ) ;
#1494 = CARTESIAN_POINT ( 'NONE',  ( -24.70764059509555111, 380.0573905601785327, 19.99999999999998934 ) ) ;
#1495 = CARTESIAN_POINT ( 'NONE',  ( -11.93348319268871727, 310.6823905683720568, -3.332260488124732856 ) ) ;
#1496 = CARTESIAN_POINT ( 'NONE',  ( -35.09675569278796559, 523.4948905683720568, -15.47720386886985544 ) ) ;
#1497 = PRESENTATION_LAYER_ASSIGNMENT (  '', '', ( #13601 ) ) ;
#1498 = CARTESIAN_POINT ( 'NONE',  ( -21.03221929538692336, 364.1198905601785327, -18.47759065022572855 ) ) ;
#1499 = EDGE_CURVE ( 'NONE', #12966, #5103, #3092, .T. ) ;
#1500 = CARTESIAN_POINT ( 'NONE',  ( -8.685887942688706786, 226.9948905765656377, -2.449293598294705724E-15 ) ) ;
#1501 = ORIENTED_EDGE ( 'NONE', *, *, #1478, .T. ) ;
#1502 = CARTESIAN_POINT ( 'NONE',  ( -25.35362745456399480, 478.1823905683720568, 16.75240474999998952 ) ) ;
#1503 = LINE ( 'NONE', #8294, #4888 ) ;
#1504 = CARTESIAN_POINT ( 'NONE',  ( -38.17536295476244845, 282.3073905683720568, -14.20200298773971426 ) ) ;
#1505 = ORIENTED_EDGE ( 'NONE', *, *, #11334, .F. ) ;
#1506 = CARTESIAN_POINT ( 'NONE',  ( -35.09675569278793716, 283.4948905683720000, -15.47720386886985544 ) ) ;
#1507 = CARTESIAN_POINT ( 'NONE',  ( -45.43829269268869808, 314.1823905683720000, 3.332260488124734632 ) ) ;
#1508 = AXIS2_PLACEMENT_3D ( 'NONE', #16904, #13343, #16588 ) ;
#1509 = CARTESIAN_POINT ( 'NONE',  ( -48.68588794268869435, 261.6823905765656377, -3.978247347593158345 ) ) ;
#1510 = FACE_OUTER_BOUND ( 'NONE', #9710, .T. ) ;
#1511 = CARTESIAN_POINT ( 'NONE',  ( -19.19641293061496157, 227.3073905683720000, 14.20200298773971426 ) ) ;
#1512 = AXIS2_PLACEMENT_3D ( 'NONE', #3268, #9843, #16788 ) ;
#1513 = CARTESIAN_POINT ( 'NONE',  ( -45.43829269268871229, 385.3698905683720568, 0.000000000000000000 ) ) ;
#1514 = ADVANCED_FACE ( 'NONE', ( #7845 ), #14474, .T. ) ;
#1515 = CARTESIAN_POINT ( 'NONE',  ( -8.685887942688887975, 281.9323905601784759, 3.978247347593586447 ) ) ;
#1516 = DIRECTION ( 'NONE',  ( 1.000000000000000000, 0.000000000000000000, -0.000000000000000000 ) ) ;
#1517 = DIRECTION ( 'NONE',  ( 1.191790137725560488E-16, -1.000000000000000000, -0.000000000000000000 ) ) ;
#1518 = B_SPLINE_CURVE_WITH_KNOTS ( 'NONE', 3,
 ( #310, #16641, #1826, #1601, #8396, #206, #5361, #19980, #20192, #18561, #11756, #3744, #6772, #6879, #21389, #10331 ),
 .UNSPECIFIED., .F., .F.,
 ( 4, 2, 2, 2, 2, 2, 2, 4 ),
 ( 0.02505096243559567018, 0.02646409050993621045, 0.02787721858427674726, 0.03070347473295781046, 0.03211660280729834727, 0.03352973088163888060, 0.03494285895597940700, 0.03635598703031994033 ),
 .UNSPECIFIED. ) ;
#1519 = CARTESIAN_POINT ( 'NONE',  ( -35.09675569278795848, 425.7448905683720000, 15.47720386886985366 ) ) ;
#1520 = FACE_OUTER_BOUND ( 'NONE', #17038, .T. ) ;
#1521 = ORIENTED_EDGE ( 'NONE', *, *, #16647, .F. ) ;
#1522 = CARTESIAN_POINT ( 'NONE',  ( -17.35679799567829917, 430.6823905601785327, 16.95518130045146421 ) ) ;
#1523 = EDGE_CURVE ( 'NONE', #16345, #880, #4712, .T. ) ;
#1524 = VERTEX_POINT ( 'NONE', #9683 ) ;
#1525 = EDGE_LOOP ( 'NONE', ( #188, #9196 ) ) ;
#1526 = ORIENTED_EDGE ( 'NONE', *, *, #9290, .F. ) ;
#1527 = LINE ( 'NONE', #9832, #3202 ) ;
#1528 = CARTESIAN_POINT ( 'NONE',  ( -32.66413529028186957, 309.4323905601784759, 19.99999999999999289 ) ) ;
#1529 = CARTESIAN_POINT ( 'NONE',  ( -42.82802356641964536, 205.1437886375728965, -5.000000000000001776 ) ) ;
#1530 = VECTOR ( 'NONE', #9051, 1000.000000000000000 ) ;
#1531 = CARTESIAN_POINT ( 'NONE',  ( -40.53162694259543741, 336.6198905683720000, 11.84573899990672885 ) ) ;
#1532 = CARTESIAN_POINT ( 'NONE',  ( -21.03221929538692692, 505.1198905765656946, 18.47759065022572500 ) ) ;
#1533 = CARTESIAN_POINT ( 'NONE',  ( -13.20868407381886023, 378.2448905683720000, 6.410867750099229490 ) ) ;
#1534 = CARTESIAN_POINT ( 'NONE',  ( -48.68588794268870146, 311.9948905765655809, 0.000000000000000000 ) ) ;
#1535 = CARTESIAN_POINT ( 'NONE',  ( -11.93348319268872437, 388.8698905683720000, -2.051577885510841163E-15 ) ) ;
#1536 = CARTESIAN_POINT ( 'NONE',  ( -11.73070664223724080, 316.0573905765655240, 11.32908994701042005 ) ) ;
#1537 = DIRECTION ( 'NONE',  ( 0.000000000000000000, 0.000000000000000000, -1.000000000000000000 ) ) ;
#1538 = CARTESIAN_POINT ( 'NONE',  ( -38.17536295476244135, 285.4323905683720568, 14.20200298773971781 ) ) ;
#1539 = CYLINDRICAL_SURFACE ( 'NONE', #18429, 125.0000000000000000 ) ;
#1540 = CARTESIAN_POINT ( 'NONE',  ( -28.68588794268872277, 432.8698905683720568, -16.75240474999999307 ) ) ;
#1541 = CARTESIAN_POINT ( 'NONE',  ( -33.84809828339280102, 56.08479096960711985, 120.3299889578561590 ) ) ;
#1542 = CARTESIAN_POINT ( 'NONE',  ( -11.73070664223726389, 501.3073905601784759, 11.32908994701042005 ) ) ;
#1543 = CARTESIAN_POINT ( 'NONE',  ( 107.6674317086782935, 187.4856410316723441, 20.00000000000000355 ) ) ;
#1544 = CARTESIAN_POINT ( 'NONE',  ( 3.458603197740078627, 160.1716627696692683, 33.59072564020503648 ) ) ;
#1545 = CARTESIAN_POINT ( 'NONE',  ( -32.01814843081344719, 347.5573905683720568, 16.75240474999999307 ) ) ;
#1546 = CARTESIAN_POINT ( 'NONE',  ( -22.27502019258950128, 490.7448905683720000, -15.47720386886985544 ) ) ;
#1547 = EDGE_LOOP ( 'NONE', ( #12729, #14512, #20221, #4392 ) ) ;
#1548 = CARTESIAN_POINT ( 'NONE',  ( -32.66413529028189089, 495.0573905601784759, -19.99999999999999289 ) ) ;
#1549 = CARTESIAN_POINT ( 'NONE',  ( -22.27502019258946930, 306.9948905683720568, 15.47720386886985189 ) ) ;
#1550 = EDGE_LOOP ( 'NONE', ( #21256, #5936, #20102 ) ) ;
#1551 = CARTESIAN_POINT ( 'NONE',  ( -36.33955658999050087, 259.1198905601784759, 18.47759065022572500 ) ) ;
#1552 = ORIENTED_EDGE ( 'NONE', *, *, #11957, .T. ) ;
#1553 = CARTESIAN_POINT ( 'NONE',  ( -18.68588794268873698, 323.8848358243226357, -20.00000000000000355 ) ) ;
#1554 = ADVANCED_FACE ( 'NONE', ( #16307 ), #14688, .F. ) ;
#1555 = EDGE_CURVE ( 'NONE', #5796, #1687, #14959, .T. ) ;
#1556 = CARTESIAN_POINT ( 'NONE',  ( -25.35362745456399836, 412.5573905683720000, -16.75240474999999307 ) ) ;
#1557 = CARTESIAN_POINT ( 'NONE',  ( -17.35679799567830273, 480.6823905601784759, 16.95518130045146421 ) ) ;
#1558 = CARTESIAN_POINT ( 'NONE',  ( 0.000000000000000000, 0.000000000000000000, 0.000000000000000000 ) ) ;
#1559 = CARTESIAN_POINT ( 'NONE',  ( -28.68588794268872277, 446.3698905683720000, 16.75240474999999307 ) ) ;
#1560 = CARTESIAN_POINT ( 'NONE',  ( -32.01814843081344719, 441.6823905683721136, -16.75240474999999307 ) ) ;
#1561 =( BOUNDED_CURVE ( )  B_SPLINE_CURVE ( 2, ( #10290, #7047, #19935, #5006, #5113, #5427, #9974, #18516, #16593, #3494, #10081, #16702, #1891, #8458, #15083, #11922, #3702 ),
 .UNSPECIFIED., .F., .T. ) 
 B_SPLINE_CURVE_WITH_KNOTS ( ( 3, 2, 2, 2, 2, 2, 2, 2, 3 ),
 ( 0.4531250000000002220, 0.4550781250000002220, 0.4570312500000002220, 0.4589843750000002220, 0.4609375000000002220, 0.4628906250000002220, 0.4648437500000002220, 0.4667968750000002220, 0.4687500000000002220 ),
 .UNSPECIFIED. ) 
 CURVE ( )  GEOMETRIC_REPRESENTATION_ITEM ( )  RATIONAL_B_SPLINE_CURVE ( ( 0.9999999999999977796, 0.9807852804032326510, 1.000000000000000000, 0.9807852804032304306, 1.000000000000000000, 0.9807852804032304306, 1.000000000000000000, 0.9807852804032304306, 1.000000000000000000, 0.9807852804032304306, 1.000000000000000000, 0.9807852804032304306, 1.000000000000000000, 0.9807852804032304306, 1.000000000000000000, 0.9807852804032282101, 1.000000000000002220 ) ) 
 REPRESENTATION_ITEM ( '' )  );
#1562 = CARTESIAN_POINT ( 'NONE',  ( 20.42502041961813930, 230.5765313837437418, -60.00000000000000000 ) ) ;
#1563 = CARTESIAN_POINT ( 'NONE',  ( -48.68588794268870856, 381.9948905765655809, 0.000000000000000000 ) ) ;
#1564 = CARTESIAN_POINT ( 'NONE',  ( -26.84549718169330035, 46.23287705007100357, 49.56899837170070811 ) ) ;
#1565 = CARTESIAN_POINT ( 'NONE',  ( -17.35679799567828496, 263.8073905601784759, -16.95518130045146421 ) ) ;
#1566 = PLANE ( 'NONE',  #2210 ) ;
#1567 = CARTESIAN_POINT ( 'NONE',  ( -28.68588794268874409, 608.2448905601786464, -20.00000000000000000 ) ) ;
#1568 = CARTESIAN_POINT ( 'NONE',  ( -44.16309181155857999, 495.9948905683720568, 6.410867750099241924 ) ) ;
#1569 = EDGE_CURVE ( 'NONE', #8426, #17432, #4112, .T. ) ;
#1570 = DIRECTION ( 'NONE',  ( -0.000000000000000000, -0.000000000000000000, 1.000000000000000000 ) ) ;
#1571 =( NAMED_UNIT ( * ) SI_UNIT ( $, .STERADIAN. ) SOLID_ANGLE_UNIT ( ) );
#1572 = CARTESIAN_POINT ( 'NONE',  ( -43.15150032496258348, 208.1972798037766950, 3.972578417695639352 ) ) ;
#1573 =( REPRESENTATION_RELATIONSHIP ('NONE','NONE', #1888, #8616 ) REPRESENTATION_RELATIONSHIP_WITH_TRANSFORMATION ( #13775 )SHAPE_REPRESENTATION_RELATIONSHIP( ) );
#1574 = EDGE_CURVE ( 'NONE', #10312, #4551, #4700, .T. ) ;
#1575 = CARTESIAN_POINT ( 'NONE',  ( -35.09675569278795138, 403.4948905683720000, -15.47720386886985544 ) ) ;
#1576 = CYLINDRICAL_SURFACE ( 'NONE', #4381, 6.500000000000000888 ) ;
#1577 = CARTESIAN_POINT ( 'NONE',  ( -38.17536295476243424, 236.9323905683720000, 14.20200298773971781 ) ) ;
#1578 = ORIENTED_EDGE ( 'NONE', *, *, #8549, .F. ) ;
#1579 = CARTESIAN_POINT ( 'NONE',  ( -40.01497788969913927, 423.5573905765656377, 16.95518130045146776 ) ) ;
#1580 = VERTEX_POINT ( 'NONE', #6972 ) ;
#1581 = CARTESIAN_POINT ( 'NONE',  ( -40.53162694259544452, 436.6198905683720000, 11.84573899990672885 ) ) ;
#1582 = CARTESIAN_POINT ( 'NONE',  ( -48.68588794268869435, 221.9948905765656377, 0.000000000000000000 ) ) ;
#1583 = EDGE_CURVE ( 'NONE', #17507, #10230, #5395, .T. ) ;
#1584 = VERTEX_POINT ( 'NONE', #15427 ) ;
#1585 = CARTESIAN_POINT ( 'NONE',  ( -48.68588794268874409, 585.7448905601785327, 2.449293598294706907E-15 ) ) ;
#1586 = CARTESIAN_POINT ( 'NONE',  ( -13.20868407381884424, 228.2448905683720568, 6.410867750099229490 ) ) ;
#1587 = VERTEX_POINT ( 'NONE', #10747 ) ;
#1588 = CARTESIAN_POINT ( 'NONE',  ( -42.88789093042844769, 502.9323905683720000, -9.489475012073734561 ) ) ;
#1589 = DIRECTION ( 'NONE',  ( -0.000000000000000000, -0.000000000000000000, 1.000000000000000000 ) ) ;
#1590 = CARTESIAN_POINT ( 'NONE',  ( -28.68588794268872633, 439.4948905765655809, -19.99999999999999289 ) ) ;
#1591 = CARTESIAN_POINT ( 'NONE',  ( -17.35679799567828852, 298.5573905765656377, -16.95518130045146421 ) ) ;
#1592 = CARTESIAN_POINT ( 'NONE',  ( -45.64106924314017277, 328.1823905601785327, 11.32908994701042538 ) ) ;
#1593 = FACE_OUTER_BOUND ( 'NONE', #14575, .T. ) ;
#1594 = DIRECTION ( 'NONE',  ( 1.374938938973709817E-16, -1.000000000000000000, 0.000000000000000000 ) ) ;
#1595 = CARTESIAN_POINT ( 'NONE',  ( 35.96497763894178945, 171.2213544847811875, -40.00000000000000000 ) ) ;
#1596 = CARTESIAN_POINT ( 'NONE',  ( -27.94030887803372210, 223.9102039777117739, 20.05120499983352289 ) ) ;
#1597 = CARTESIAN_POINT ( 'NONE',  ( -14.54375231895778420, 495.7448905765656377, 14.14213562373094568 ) ) ;
#1598 = CARTESIAN_POINT ( 'NONE',  ( -45.43829269268870519, 325.3698905683720000, 0.000000000000000000 ) ) ;
#1599 = CARTESIAN_POINT ( 'NONE',  ( -48.68588794268869435, 237.2448905601785043, 0.000000000000000000 ) ) ;
#1600 = CARTESIAN_POINT ( 'NONE',  ( -11.73070664223723725, 263.1823905601784759, -11.32908994701042715 ) ) ;
#1601 = CARTESIAN_POINT ( 'NONE',  ( -30.17610990746410593, 48.40110735202731718, -49.57983718523864525 ) ) ;
#1602 = CARTESIAN_POINT ( 'NONE',  ( -19.19641293061497578, 288.8073905683719431, 14.20200298773971426 ) ) ;
#1603 = EDGE_CURVE ( 'NONE', #3040, #19138, #13575, .T. ) ;
#1604 = CARTESIAN_POINT ( 'NONE',  ( -28.68588794268873343, 527.8698905683720568, 16.75240474999999307 ) ) ;
#1605 = CARTESIAN_POINT ( 'NONE',  ( -14.54375231895776821, 370.9948905601784759, 14.14213562373094568 ) ) ;
#1606 = AXIS2_PLACEMENT_3D ( 'NONE', #144, #11590, #1439 ) ;
#1607 = CARTESIAN_POINT ( 'NONE',  ( -45.64106924314017277, 316.3073905601785327, -11.32908994701042538 ) ) ;
#1608 = VERTEX_POINT ( 'NONE', #20824 ) ;
#1609 = CARTESIAN_POINT ( 'NONE',  ( -13.20868407381887621, 490.9948905683720568, -6.410867750099233042 ) ) ;
#1610 = DIRECTION ( 'NONE',  ( 0.000000000000000000, 1.000000000000000000, -0.000000000000000000 ) ) ;
#1611 = CARTESIAN_POINT ( 'NONE',  ( -14.48388495494899075, 289.8073905683720000, -9.489475012073736337 ) ) ;
#1612 = ORIENTED_EDGE ( 'NONE', *, *, #10926, .F. ) ;
#1613 = CARTESIAN_POINT ( 'NONE',  ( -40.01497788969911795, 228.8073905601784475, 16.95518130045146776 ) ) ;
#1614 = CARTESIAN_POINT ( 'NONE',  ( -45.43829269268870519, 275.3698905683720000, 0.000000000000000000 ) ) ;
#1615 = AXIS2_PLACEMENT_3D ( 'NONE', #7084, #16849, #18241 ) ;
#1616 = CARTESIAN_POINT ( 'NONE',  ( -45.43829269268869808, 265.3698905683720000, 0.000000000000000000 ) ) ;
#1617 = CARTESIAN_POINT ( 'NONE',  ( -11.73070664223723547, 237.9323905765656093, -11.32908994701042715 ) ) ;
#1618 = CARTESIAN_POINT ( 'NONE',  ( -45.64106924314019409, 476.3073905601785327, -11.32908994701042538 ) ) ;
#1619 = CARTESIAN_POINT ( 'NONE',  ( -16.84014894278196905, 227.6198905683720000, 11.84573899990672530 ) ) ;
#1620 = CARTESIAN_POINT ( 'NONE',  ( -16.84014894278197616, 267.6198905683720568, 11.84573899990672530 ) ) ;
#1621 = CARTESIAN_POINT ( 'NONE',  ( -35.09675569278794427, 383.4948905683720000, -15.47720386886985544 ) ) ;
#1622 = EDGE_CURVE ( 'NONE', #20443, #21097, #12171, .T. ) ;
#1623 = VECTOR ( 'NONE', #9251, 1000.000000000000000 ) ;
#1624 = DIRECTION ( 'NONE',  ( -0.000000000000000000, 1.000000000000000000, -0.000000000000000000 ) ) ;
#1625 = DIRECTION ( 'NONE',  ( -0.000000000000000000, 0.000000000000000000, -1.000000000000000000 ) ) ;
#1626 = CARTESIAN_POINT ( 'NONE',  ( -8.685887942688712116, 266.9948905765656377, -2.449293598294705724E-15 ) ) ;
#1627 = CIRCLE ( 'NONE', #5407, 20.00000000000000355 ) ;
#1628 = CARTESIAN_POINT ( 'NONE',  ( -42.88789093042844058, 414.8073905683720568, 9.489475012073736337 ) ) ;
#1629 = PRODUCT_RELATED_PRODUCT_CATEGORY ( 'part', '', ( #19255 ) ) ;
#1630 = CARTESIAN_POINT ( 'NONE',  ( -28.68588794268874054, 573.2448905601785327, 0.000000000000000000 ) ) ;
#1631 = ORIENTED_EDGE ( 'NONE', *, *, #15630, .T. ) ;
#1632 = CARTESIAN_POINT ( 'NONE',  ( -32.66413529028188378, 419.4323905601784190, 19.99999999999999289 ) ) ;
#1633 = ORIENTED_EDGE ( 'NONE', *, *, #5512, .T. ) ;
#1634 = CARTESIAN_POINT ( 'NONE',  ( 105.7989814974898479, 142.5259582928263455, -40.00000000000000000 ) ) ;
#1635 = ORIENTED_EDGE ( 'NONE', *, *, #6501, .F. ) ;
#1636 = FACE_OUTER_BOUND ( 'NONE', #14623, .T. ) ;
#1637 = CARTESIAN_POINT ( 'NONE',  ( -28.68588794268870501, 299.7448905601784759, 19.99999999999999289 ) ) ;
#1638 = FACE_BOUND ( 'NONE', #1135, .T. ) ;
#1639 = ADVANCED_FACE ( 'NONE', ( #17362 ), #4374, .F. ) ;
#1640 = CARTESIAN_POINT ( 'NONE',  ( -32.01814843081344719, 347.5573905683720568, 16.75240474999999307 ) ) ;
#1641 = AXIS2_PLACEMENT_3D ( 'NONE', #2977, #9555, #19198 ) ;
#1642 = CARTESIAN_POINT ( 'NONE',  ( -24.70764059509557953, 489.1823905765656377, -19.99999999999999289 ) ) ;
#1643 = CARTESIAN_POINT ( 'NONE',  ( -22.27502019258948707, 370.7448905683720568, -15.47720386886985544 ) ) ;
#1644 = CARTESIAN_POINT ( 'NONE',  ( -32.01814843081343298, 223.1823905683720000, -16.75240474999999307 ) ) ;
#1645 = CARTESIAN_POINT ( 'NONE',  ( -32.01814843081344719, 396.0573905683720568, 16.75240474999999307 ) ) ;
#1646 = VECTOR ( 'NONE', #9638, 1000.000000000000114 ) ;
#1647 = CARTESIAN_POINT ( 'NONE',  ( -48.68588794268870146, 301.9948905765655809, 0.000000000000000000 ) ) ;
#1648 = CARTESIAN_POINT ( 'NONE',  ( 52.60622592008805043, 30.52886280891152282, -151.0302712373927250 ) ) ;
#1649 = CARTESIAN_POINT ( 'NONE',  ( -16.84014894278197616, 277.6198905683720568, 11.84573899990672530 ) ) ;
#1650 = CARTESIAN_POINT ( 'NONE',  ( 6.416697501590670427, 217.7548513357008630, 49.99999999999999289 ) ) ;
#1651 = CARTESIAN_POINT ( 'NONE',  ( -44.16309181155857289, 435.9948905683720568, 6.410867750099241924 ) ) ;
#1652 = EDGE_CURVE ( 'NONE', #9090, #12399, #581, .T. ) ;
#1653 = DIRECTION ( 'NONE',  ( 0.000000000000000000, -0.000000000000000000, 1.000000000000000000 ) ) ;
#1654 = EDGE_CURVE ( 'NONE', #5794, #9671, #20601, .T. ) ;
#1655 = CARTESIAN_POINT ( 'NONE',  ( -32.66413529028188378, 499.4323905601784759, 19.99999999999999289 ) ) ;
#1656 = CARTESIAN_POINT ( 'NONE',  ( 21.30000000000000071, 0.000000000000000000, 0.000000000000000000 ) ) ;
#1657 = UNCERTAINTY_MEASURE_WITH_UNIT (LENGTH_MEASURE( 1.000000000000000082E-05 ), #14638, 'distance_accuracy_value', 'NONE');
#1658 = CARTESIAN_POINT ( 'NONE',  ( -10.20829729246299600, 451.6198905601784759, 7.653668647301790529 ) ) ;
#1659 = CARTESIAN_POINT ( 'NONE',  ( -40.53162694259543741, 344.1198905683720568, -11.84573899990672707 ) ) ;
#1660 = CARTESIAN_POINT ( 'NONE',  ( -38.17536295476246977, 482.3073905683720568, -14.20200298773971426 ) ) ;
#1661 = ORIENTED_EDGE ( 'NONE', *, *, #1693, .T. ) ;
#1662 = CARTESIAN_POINT ( 'NONE',  ( -36.33955658999052929, 489.1198905601785327, 18.47759065022572500 ) ) ;
#1663 = CARTESIAN_POINT ( 'NONE',  ( -16.84014894278197971, 307.6198905683720000, 11.84573899990672530 ) ) ;
#1664 = ORIENTED_EDGE ( 'NONE', *, *, #10335, .F. ) ;
#1665 = CARTESIAN_POINT ( 'NONE',  ( -42.82802356641965957, 343.2448905765656377, 14.14213562373094923 ) ) ;
#1666 = PRODUCT_DEFINITION_SHAPE ( 'NONE', 'NONE',  #11071 ) ;
#1667 = ORIENTED_EDGE ( 'NONE', *, *, #5396, .T. ) ;
#1668 = LINE ( 'NONE', #2964, #11883 ) ;
#1669 = CARTESIAN_POINT ( 'NONE',  ( -38.17536295476245556, 406.9323905683719431, 14.20200298773971781 ) ) ;
#1670 = DIRECTION ( 'NONE',  ( 0.8865057725575725689, 0.000000000000000000, 0.4627175328665443232 ) ) ;
#1671 = CARTESIAN_POINT ( 'NONE',  ( -42.88789093042844058, 424.8073905683720000, 9.489475012073736337 ) ) ;
#1672 = CARTESIAN_POINT ( 'NONE',  ( -22.27502019258949773, 440.7448905683720000, -15.47720386886985544 ) ) ;
#1673 = CARTESIAN_POINT ( 'NONE',  ( -32.66413529028187668, 399.4323905601784759, 19.99999999999999289 ) ) ;
#1674 = CARTESIAN_POINT ( 'NONE',  ( -17.35679799567829562, 375.4323905765656377, 16.95518130045146421 ) ) ;
#1675 = CARTESIAN_POINT ( 'NONE',  ( -11.33448572641403906, 53.24576043933482339, 46.46721659624293466 ) ) ;
#1676 = PLANE ( 'NONE',  #10600 ) ;
#1677 = DIRECTION ( 'NONE',  ( 1.000000000000000000, 0.000000000000000000, -0.000000000000000000 ) ) ;
#1678 = CARTESIAN_POINT ( 'NONE',  ( -48.68588794268872277, 491.9948905765656377, 0.000000000000000000 ) ) ;
#1679 = CARTESIAN_POINT ( 'NONE',  ( -28.68588794268873343, 492.8698905683720568, -16.75240474999999307 ) ) ;
#1680 = DIRECTION ( 'NONE',  ( 0.02283316540262222277, -0.9997392892938120612, -0.000000000000000000 ) ) ;
#1681 = DIRECTION ( 'NONE',  ( -1.191790137725560488E-16, 1.000000000000000000, -0.000000000000000000 ) ) ;
#1682 = CARTESIAN_POINT ( 'NONE',  ( 20.60949999999999349, 4.898587196589412829E-16, -4.000000000000000000 ) ) ;
#1683 = CARTESIAN_POINT ( 'NONE',  ( -40.53162694259544452, 406.6198905683720568, 11.84573899990672885 ) ) ;
#1684 = CARTESIAN_POINT ( 'NONE',  ( -11.73070664223726389, 467.9323905765655240, -11.32908994701042538 ) ) ;
#1685 = CARTESIAN_POINT ( 'NONE',  ( -40.53162694259542320, 234.1198905683720000, -11.84573899990672707 ) ) ;
#1686 = VECTOR ( 'NONE', #12723, 1000.000000000000000 ) ;
#1687 = VERTEX_POINT ( 'NONE', #18757 ) ;
#1688 = CARTESIAN_POINT ( 'NONE',  ( -21.03221929538691626, 425.1198905765656377, 18.47759065022572500 ) ) ;
#1689 = ORIENTED_EDGE ( 'NONE', *, *, #11921, .T. ) ;
#1690 = CARTESIAN_POINT ( 'NONE',  ( -42.88789093042844058, 434.4323905683720568, -9.489475012073734561 ) ) ;
#1691 =( BOUNDED_CURVE ( )  B_SPLINE_CURVE ( 3, ( #8667, #10181, #15291, #15395 ),
 .UNSPECIFIED., .F., .T. ) 
 B_SPLINE_CURVE_WITH_KNOTS ( ( 4, 4 ),
 ( 3.164427803482926738, 4.453488305187281782 ),
 .UNSPECIFIED. ) 
 CURVE ( )  GEOMETRIC_REPRESENTATION_ITEM ( )  RATIONAL_B_SPLINE_CURVE ( ( 1.000000000000000000, 0.8662547274802335773, 0.8662547274802335773, 1.000000000000000000 ) ) 
 REPRESENTATION_ITEM ( '' )  );
#1692 = CARTESIAN_POINT ( 'NONE',  ( -22.27502019258950483, 520.7448905683720568, -15.47720386886985544 ) ) ;
#1693 = EDGE_CURVE ( 'NONE', #5209, #6118, #4155, .T. ) ;
#1694 = ORIENTED_EDGE ( 'NONE', *, *, #5982, .T. ) ;
#1695 = CARTESIAN_POINT ( 'NONE',  ( -42.82802356641965247, 205.4732429224858095, 5.000000000000000888 ) ) ;
#1696 = CARTESIAN_POINT ( 'NONE',  ( -35.09675569278796559, 533.4948905683720568, -15.47720386886985544 ) ) ;
#1697 = EDGE_CURVE ( 'NONE', #18805, #19193, #17964, .T. ) ;
#1698 = ORIENTED_EDGE ( 'NONE', *, *, #13300, .F. ) ;
#1699 = CARTESIAN_POINT ( 'NONE',  ( -22.27502019258950128, 500.7448905683720000, -15.47720386886985544 ) ) ;
#1700 = CARTESIAN_POINT ( 'NONE',  ( -24.08721141673526489, 45.45117433463647671, -49.38795028004579990 ) ) ;
#1701 = ADVANCED_FACE ( 'NONE', ( #1244 ), #11067, .T. ) ;
#1702 = CARTESIAN_POINT ( 'NONE',  ( -10.20829729246299600, 446.3698905765656377, 7.653668647301790529 ) ) ;
#1703 = DIRECTION ( 'NONE',  ( -1.000000000000000000, 0.000000000000000000, 0.000000000000000000 ) ) ;
#1704 = CARTESIAN_POINT ( 'NONE',  ( -24.70764059509554755, 330.0573905601785896, 19.99999999999998934 ) ) ;
#1705 = DIRECTION ( 'NONE',  ( -1.000000000000000000, -0.000000000000000000, -0.000000000000000000 ) ) ;
#1706 = APPLICATION_CONTEXT ( 'automotive_design' ) ;
#1707 = DIRECTION ( 'NONE',  ( 1.000000000000000000, 0.000000000000000000, 0.000000000000000000 ) ) ;
#1708 = CARTESIAN_POINT ( 'NONE',  ( -28.68588794268873698, 56.85652257517428865, 0.000000000000000000 ) ) ;
#1709 = CARTESIAN_POINT ( 'NONE',  ( 35.96497763894178945, 171.2213544847811875, 40.00000000000000000 ) ) ;
#1710 = CARTESIAN_POINT ( 'NONE',  ( -43.67481775055303928, 200.1767262095909246, -0.6600471188826696478 ) ) ;
#1711 = CARTESIAN_POINT ( 'NONE',  ( -19.19641293061497578, 298.8073905683719431, 14.20200298773971426 ) ) ;
#1712 = EDGE_CURVE ( 'NONE', #1687, #15268, #14346, .T. ) ;
#1713 = CARTESIAN_POINT ( 'NONE',  ( -13.68588794268869790, 213.9102039777116602, 1.836970198721029589E-15 ) ) ;
#1714 = CARTESIAN_POINT ( 'NONE',  ( -32.66413529028186247, 259.4323905601784759, 19.99999999999999289 ) ) ;
#1715 = CARTESIAN_POINT ( 'NONE',  ( -17.35679799567829562, 415.4323905765656946, 16.95518130045146421 ) ) ;
#1716 = CARTESIAN_POINT ( 'NONE',  ( -22.27502019258946930, 298.4948905683720568, 15.47720386886985189 ) ) ;
#1717 = CARTESIAN_POINT ( 'NONE',  ( -11.93348319268873858, 500.6823905683720568, -3.332260488124732856 ) ) ;
#1718 = CARTESIAN_POINT ( 'NONE',  ( -36.33955658999050797, 365.3698905601784759, -18.47759065022572855 ) ) ;
#1719 = VECTOR ( 'NONE', #13753, 1000.000000000000000 ) ;
#1720 = ORIENTED_EDGE ( 'NONE', *, *, #18947, .T. ) ;
#1721 = CARTESIAN_POINT ( 'NONE',  ( -32.01814843081346140, 463.1823905683720000, -16.75240474999999307 ) ) ;
#1722 = CARTESIAN_POINT ( 'NONE',  ( 158.8141120573112630, 575.7448905601785327, 0.000000000000000000 ) ) ;
#1723 = CARTESIAN_POINT ( 'NONE',  ( -19.19641293061497223, 277.3073905683720000, 14.20200298773971426 ) ) ;
#1724 = ORIENTED_EDGE ( 'NONE', *, *, #9819, .T. ) ;
#1725 = CARTESIAN_POINT ( 'NONE',  ( -48.68588794268869435, 227.2448905601785043, 0.000000000000000000 ) ) ;
#1726 = CARTESIAN_POINT ( 'NONE',  ( -11.93348319268871194, 280.6823905683720000, -3.332260488124732856 ) ) ;
#1727 = CARTESIAN_POINT ( 'NONE',  ( -44.16309181155855157, 255.9948905683720568, 6.410867750099241924 ) ) ;
#1728 = CARTESIAN_POINT ( 'NONE',  ( -32.66413529028186247, 249.8073905765656662, -19.99999999999999289 ) ) ;
#1729 = CARTESIAN_POINT ( 'NONE',  ( -14.54375231895777709, 418.2448905765655809, -14.14213562373094746 ) ) ;
#1730 = CARTESIAN_POINT ( 'NONE',  ( -24.70764059509552979, 230.0573905601784759, 19.99999999999998934 ) ) ;
#1731 = CARTESIAN_POINT ( 'NONE',  ( -71.26501780185373036, 213.9102039777116602, 0.000000000000000000 ) ) ;
#1732 = CARTESIAN_POINT ( 'NONE',  ( -32.01814843081343298, 261.6823905683720568, -16.75240474999999307 ) ) ;
#1733 = CARTESIAN_POINT ( 'NONE',  ( -11.93348319268872260, 370.0573905683719431, 3.332260488124728415 ) ) ;
#1734 = VECTOR ( 'NONE', #20383, 1000.000000000000000 ) ;
#1735 = CARTESIAN_POINT ( 'NONE',  ( -43.60108677734861260, 200.4027425691367057, 1.621665263882683838 ) ) ;
#1736 = DIRECTION ( 'NONE',  ( 0.000000000000000000, 0.000000000000000000, -1.000000000000000000 ) ) ;
#1737 = DIRECTION ( 'NONE',  ( -1.000000000000000000, -0.000000000000000000, -0.000000000000000000 ) ) ;
#1738 = CARTESIAN_POINT ( 'NONE',  ( -28.68588794268872277, 421.3698905683720568, -16.75240474999999307 ) ) ;
#1739 = PLANE ( 'NONE',  #512 ) ;
#1740 = ORIENTED_EDGE ( 'NONE', *, *, #8071, .T. ) ;
#1741 = CARTESIAN_POINT ( 'NONE',  ( -48.68588794268871567, 427.2448905601784759, 0.000000000000000000 ) ) ;
#1742 = ORIENTED_EDGE ( 'NONE', *, *, #6387, .F. ) ;
#1743 = DIRECTION ( 'NONE',  ( -1.000000000000000000, -0.000000000000000000, -0.000000000000000000 ) ) ;
#1744 = ORIENTED_EDGE ( 'NONE', *, *, #18262, .T. ) ;
#1745 = ORIENTED_EDGE ( 'NONE', *, *, #3500, .T. ) ;
#1746 = CARTESIAN_POINT ( 'NONE',  ( -21.03221929538690915, 355.1198905765656377, 18.47759065022572500 ) ) ;
#1747 = CARTESIAN_POINT ( 'NONE',  ( -14.54375231895775933, 310.9948905601784759, 14.14213562373094568 ) ) ;
#1748 = FACE_BOUND ( 'NONE', #6583, .T. ) ;
#1749 = EDGE_CURVE ( 'NONE', #534, #16560, #6200, .T. ) ;
#1750 = CARTESIAN_POINT ( 'NONE',  ( -42.88789093042843348, 344.4323905683719431, -9.489475012073734561 ) ) ;
#1751 = CIRCLE ( 'NONE', #2104, 38.00000000000000000 ) ;
#1752 = ORIENTED_EDGE ( 'NONE', *, *, #20775, .T. ) ;
#1753 = CARTESIAN_POINT ( 'NONE',  ( -45.64106924314020119, 482.9323905765656377, 11.32908994701042715 ) ) ;
#1754 = CARTESIAN_POINT ( 'NONE',  ( -11.93348319268872260, 368.5573905683720568, 3.332260488124728415 ) ) ;
#1755 = CARTESIAN_POINT ( 'NONE',  ( -44.16309181155857999, 393.2448905683720568, -6.410867750099231266 ) ) ;
#1756 = VECTOR ( 'NONE', #4073, 1000.000000000000000 ) ;
#1757 = CARTESIAN_POINT ( 'NONE',  ( -48.68588794268870146, 302.3073905765655809, 3.978247347593168115 ) ) ;
#1758 = PLANE ( 'NONE',  #686 ) ;
#1759 = EDGE_CURVE ( 'NONE', #5272, #15608, #7604, .T. ) ;
#1760 = CARTESIAN_POINT ( 'NONE',  ( -38.17536295476244135, 295.4323905683720000, 14.20200298773971781 ) ) ;
#1761 = CARTESIAN_POINT ( 'NONE',  ( -10.20829729246299422, 441.6198905601784759, 7.653668647301790529 ) ) ;
#1762 = CLOSED_SHELL ( 'NONE', ( #4254, #7700, #10763, #5705, #463, #10790, #10403, #16061, #9033, #19364, #19712, #8820, #7218, #3065, #7846, #20538, #4593, #3084, #19659 ) ) ;
#1763 = CARTESIAN_POINT ( 'NONE',  ( -25.35362745456398770, 428.1823905683720000, 16.75240474999998952 ) ) ;
#1764 = DIRECTION ( 'NONE',  ( 0.000000000000000000, 1.000000000000000000, 0.000000000000000000 ) ) ;
#1765 = CARTESIAN_POINT ( 'NONE',  ( -47.16347859291445843, 497.8698905601784759, 7.653668647301805628 ) ) ;
#1766 = FACE_OUTER_BOUND ( 'NONE', #2668, .T. ) ;
#1767 = VECTOR ( 'NONE', #17389, 1000.000000000000000 ) ;
#1768 = DIRECTION ( 'NONE',  ( 0.000000000000000000, 0.000000000000000000, 1.000000000000000000 ) ) ;
#1769 = CARTESIAN_POINT ( 'NONE',  ( -13.20868407381885667, 349.7448905683720568, 6.410867750099229490 ) ) ;
#1770 = CARTESIAN_POINT ( 'NONE',  ( -38.17536295476246266, 485.4323905683720000, 14.20200298773971781 ) ) ;
#1771 = EDGE_LOOP ( 'NONE', ( #6459, #8341, #11486, #9330 ) ) ;
#1772 = CARTESIAN_POINT ( 'NONE',  ( -8.685887942688735208, 482.2448905601784759, -2.449293598294705724E-15 ) ) ;
#1773 = CARTESIAN_POINT ( 'NONE',  ( -19.19641293061497578, 307.3073905683720000, 14.20200298773971426 ) ) ;
#1774 = ORIENTED_EDGE ( 'NONE', *, *, #5730, .T. ) ;
#1775 = VECTOR ( 'NONE', #9135, 1000.000000000000000 ) ;
#1776 = AXIS2_PLACEMENT_3D ( 'NONE', #17630, #12444, #5836 ) ;
#1777 = LINE ( 'NONE', #19930, #14643 ) ;
#1778 = ORIENTED_EDGE ( 'NONE', *, *, #18591, .F. ) ;
#1779 = LINE ( 'NONE', #3064, #14329 ) ;
#1780 = EDGE_CURVE ( 'NONE', #3413, #8877, #19299, .T. ) ;
#1781 = CARTESIAN_POINT ( 'NONE',  ( -40.53162694259544452, 396.6198905683720568, 11.84573899990672885 ) ) ;
#1782 = CARTESIAN_POINT ( 'NONE',  ( -8.685887942688726326, 386.9948905765655809, -2.449293598294705724E-15 ) ) ;
#1783 = CARTESIAN_POINT ( 'NONE',  ( -42.88789093042844058, 414.8073905683720568, 9.489475012073736337 ) ) ;
#1784 = CARTESIAN_POINT ( 'NONE',  ( -16.84014894278197616, 259.1198905683720568, 11.84573899990672530 ) ) ;
#1785 = AXIS2_PLACEMENT_3D ( 'NONE', #13720, #18253, #535 ) ;
#1786 = CARTESIAN_POINT ( 'NONE',  ( -13.20868407381886733, 438.2448905683720000, 6.410867750099229490 ) ) ;
#1787 = DIRECTION ( 'NONE',  ( -0.8755316792554366234, 0.4831607171740635587, 0.000000000000000000 ) ) ;
#1788 = CARTESIAN_POINT ( 'NONE',  ( 4.700000000000000178, 0.000000000000000000, 6.500000000000000888 ) ) ;
#1789 = CARTESIAN_POINT ( 'NONE',  ( -45.64106924314018698, 371.0573905765656377, -11.32908994701042715 ) ) ;
#1790 = CARTESIAN_POINT ( 'NONE',  ( 30.42502041961814996, 180.1716627696692967, 20.00000000000000355 ) ) ;
#1791 = CARTESIAN_POINT ( 'NONE',  ( -21.03221929538692692, 388.8698905765656377, -18.47759065022572855 ) ) ;
#1792 = PLANE ( 'NONE',  #7361 ) ;
#1793 = FACE_OUTER_BOUND ( 'NONE', #19145, .T. ) ;
#1794 = CARTESIAN_POINT ( 'NONE',  ( -13.20868407381887799, 500.9948905683721136, -6.410867750099233042 ) ) ;
#1795 = AXIS2_PLACEMENT_3D ( 'NONE', #14944, #16457, #6701 ) ;
#1796 = DIRECTION ( 'NONE',  ( -0.3090169943749473402, 0.000000000000000000, -0.9510565162951535312 ) ) ;
#1797 = CARTESIAN_POINT ( 'NONE',  ( -8.685887942688580665, 462.5573905601784759, -3.978247347592792860 ) ) ;
#1798 = CARTESIAN_POINT ( 'NONE',  ( -43.47642916300955562, 209.4785612017895176, 2.513052019990858366 ) ) ;
#1799 = ADVANCED_FACE ( 'NONE', ( #2762 ), #9339, .F. ) ;
#1800 = CARTESIAN_POINT ( 'NONE',  ( -14.48388495494900496, 409.4323905683720000, 9.489475012073732785 ) ) ;
#1801 = CARTESIAN_POINT ( 'NONE',  ( -23.81231864750899874, 45.39031082328558853, -122.7132075424382975 ) ) ;
#1802 = CARTESIAN_POINT ( 'NONE',  ( -28.68588794268870146, 232.8698905683720284, -16.75240474999999307 ) ) ;
#1803 = CARTESIAN_POINT ( 'NONE',  ( -25.35362745456399125, 371.0573905683720000, -16.75240474999999307 ) ) ;
#1804 = ORIENTED_EDGE ( 'NONE', *, *, #440, .F. ) ;
#1805 = CARTESIAN_POINT ( 'NONE',  ( -28.68588794268873698, 521.3698905683720568, -16.75240474999999307 ) ) ;
#1806 = ORIENTED_EDGE ( 'NONE', *, *, #12490, .T. ) ;
#1807 = CARTESIAN_POINT ( 'NONE',  ( -13.20868407381887089, 440.9948905683720568, -6.410867750099233042 ) ) ;
#1808 = CARTESIAN_POINT ( 'NONE',  ( -44.16309181155858710, 524.4948905683719431, 6.410867750099241924 ) ) ;
#1809 = EDGE_CURVE ( 'NONE', #3125, #16161, #3183, .T. ) ;
#1810 = CARTESIAN_POINT ( 'NONE',  ( 20.42502041961813575, 271.1055109169419666, 20.00000000000000355 ) ) ;
#1811 = CARTESIAN_POINT ( 'NONE',  ( -24.70764059509555466, 430.0573905601785327, 19.99999999999998934 ) ) ;
#1812 = CARTESIAN_POINT ( 'NONE',  ( -32.01814843081346140, 491.6823905683720000, -16.75240474999999307 ) ) ;
#1813 = AXIS2_PLACEMENT_3D ( 'NONE', #1052, #21250, #21037 ) ;
#1814 = VERTEX_POINT ( 'NONE', #1145 ) ;
#1815 = CARTESIAN_POINT ( 'NONE',  ( -19.19641293061499709, 497.3073905683721136, 14.20200298773971426 ) ) ;
#1816 = CARTESIAN_POINT ( 'NONE',  ( -162.2727221670389781, 30.52886280891152282, 0.000000000000000000 ) ) ;
#1817 = CARTESIAN_POINT ( 'NONE',  ( -17.35679799567829917, 425.4323905765656377, 16.95518130045146421 ) ) ;
#1818 = CARTESIAN_POINT ( 'NONE',  ( -32.66413529028186247, 299.8073905765656377, -19.99999999999999289 ) ) ;
#1819 = CARTESIAN_POINT ( 'NONE',  ( -32.66413529028186247, 329.4323905601784759, 19.99999999999999289 ) ) ;
#1820 = FACE_OUTER_BOUND ( 'NONE', #12158, .T. ) ;
#1821 = CARTESIAN_POINT ( 'NONE',  ( -28.68588794268873698, 10.52886280891152104, 49.60091809715359545 ) ) ;
#1822 = CARTESIAN_POINT ( 'NONE',  ( -36.33955658999052929, 493.8698905765655809, 18.47759065022572500 ) ) ;
#1823 = CARTESIAN_POINT ( 'NONE',  ( -11.93348319268871371, 290.6823905683721136, -3.332260488124732856 ) ) ;
#1824 = CARTESIAN_POINT ( 'NONE',  ( -28.68588794268870146, 234.7448905601785043, -19.99999999999999289 ) ) ;
#1825 = CARTESIAN_POINT ( 'NONE',  ( -24.70764059509555111, 264.4323905601784759, -19.99999999999999289 ) ) ;
#1826 = CARTESIAN_POINT ( 'NONE',  ( -29.45535109478274549, 47.78365127927891365, -49.59625936778542155 ) ) ;
#1827 = MECHANICAL_DESIGN_GEOMETRIC_PRESENTATION_REPRESENTATION (  '', ( #4219 ), #20805 ) ;
#1828 = CARTESIAN_POINT ( 'NONE',  ( -45.43829269268869808, 285.0573905683720000, -3.332260488124726194 ) ) ;
#1829 = CARTESIAN_POINT ( 'NONE',  ( -8.685887942688442109, 532.5573905601785327, -3.978247347592446914 ) ) ;
#1830 = CARTESIAN_POINT ( 'NONE',  ( -11.93348319268873858, 510.6823905683719431, -3.332260488124732856 ) ) ;
#1831 = CARTESIAN_POINT ( 'NONE',  ( 65.85920792673738333, 160.1716627696692683, 20.00000000000000355 ) ) ;
#1832 = ORIENTED_EDGE ( 'NONE', *, *, #16714, .F. ) ;
#1833 = CARTESIAN_POINT ( 'NONE',  ( -25.35362745456400191, 462.5573905683720000, -16.75240474999999307 ) ) ;
#1834 = CARTESIAN_POINT ( 'NONE',  ( 78.68120802659203150, 149.7457237375499517, 94.99999999999994316 ) ) ;
#1835 = CARTESIAN_POINT ( 'NONE',  ( -25.35362745456396993, 266.6823905683720568, 16.75240474999998952 ) ) ;
#1836 = EDGE_CURVE ( 'NONE', #13685, #16081, #21242, .T. ) ;
#1837 = VECTOR ( 'NONE', #6097, 1000.000000000000000 ) ;
#1838 = ORIENTED_EDGE ( 'NONE', *, *, #16152, .T. ) ;
#1839 = CARTESIAN_POINT ( 'NONE',  ( 71.23374292195468627, 79.16544270676153872, -94.99999999999994316 ) ) ;
#1840 = ADVANCED_FACE ( 'NONE', ( #19613 ), #21029, .T. ) ;
#1841 = CARTESIAN_POINT ( 'NONE',  ( -11.93348319268871016, 270.0573905683719431, 3.332260488124728859 ) ) ;
#1842 = CARTESIAN_POINT ( 'NONE',  ( -16.84014894278197261, 239.1198905683720284, 11.84573899990672530 ) ) ;
#1843 = CARTESIAN_POINT ( 'NONE',  ( -40.01497788969912506, 250.4323905765656093, -16.95518130045146421 ) ) ;
#1844 = CARTESIAN_POINT ( 'NONE',  ( 170.2047888904039610, 610.7448905601785327, -1.893624729818132124 ) ) ;
#1845 = CARTESIAN_POINT ( 'NONE',  ( -32.66413529028186247, 225.0573905601784759, -19.99999999999999289 ) ) ;
#1846 = CARTESIAN_POINT ( 'NONE',  ( 1.336753550880579347E-14, 213.9102039777116602, 25.00000000000000000 ) ) ;
#1847 = CARTESIAN_POINT ( 'NONE',  ( -35.09675569278793006, 261.9948905683720000, -15.47720386886985544 ) ) ;
#1848 = CARTESIAN_POINT ( 'NONE',  ( -38.17536295476244845, 356.9323905683720000, 14.20200298773971781 ) ) ;
#1849 = DIRECTION ( 'NONE',  ( -1.191790137725560488E-16, 1.000000000000000000, -0.000000000000000000 ) ) ;
#1850 = DIRECTION ( 'NONE',  ( 0.000000000000000000, 0.000000000000000000, -1.000000000000000000 ) ) ;
#1851 = CIRCLE ( 'NONE', #5281, 50.00000000000000000 ) ;
#1852 = CARTESIAN_POINT ( 'NONE',  ( -13.20868407381886733, 419.4948905683720000, -6.410867750099233042 ) ) ;
#1853 = CARTESIAN_POINT ( 'NONE',  ( -42.82802356641965957, 340.7448905765655809, -14.14213562373094746 ) ) ;
#1854 = ORIENTED_EDGE ( 'NONE', *, *, #18917, .F. ) ;
#1855 = CARTESIAN_POINT ( 'NONE',  ( -14.54375231895777176, 410.9948905601785327, 14.14213562373094568 ) ) ;
#1856 = ORIENTED_EDGE ( 'NONE', *, *, #19326, .F. ) ;
#1857 = CARTESIAN_POINT ( 'NONE',  ( 4.700000000000000178, 0.000000000000000000, 0.000000000000000000 ) ) ;
#1858 = VERTEX_POINT ( 'NONE', #4586 ) ;
#1859 = CARTESIAN_POINT ( 'NONE',  ( -19.19641293061500065, 528.8073905683719431, 14.20200298773971426 ) ) ;
#1860 = CARTESIAN_POINT ( 'NONE',  ( -21.03221929538691626, 314.1198905601784759, -18.47759065022572855 ) ) ;
#1861 = DIRECTION ( 'NONE',  ( 0.000000000000000000, 0.000000000000000000, 1.000000000000000000 ) ) ;
#1862 = CIRCLE ( 'NONE', #3905, 9.999999999999994671 ) ;
#1863 = CARTESIAN_POINT ( 'NONE',  ( -19.19641293061497933, 321.9323905683720568, -14.20200298773971603 ) ) ;
#1864 = ORIENTED_EDGE ( 'NONE', *, *, #2046, .F. ) ;
#1865 = CARTESIAN_POINT ( 'NONE',  ( -14.48388495494900141, 369.8073905683720000, -9.489475012073736337 ) ) ;
#1866 = AXIS2_PLACEMENT_3D ( 'NONE', #11748, #1705, #13278 ) ;
#1867 = CARTESIAN_POINT ( 'NONE',  ( -14.48388495494899963, 359.8073905683720000, -9.489475012073734561 ) ) ;
#1868 = CARTESIAN_POINT ( 'NONE',  ( -48.68588794268870146, 311.6823905765656377, -3.978247347593158345 ) ) ;
#1869 = FACE_OUTER_BOUND ( 'NONE', #4529, .T. ) ;
#1870 = CARTESIAN_POINT ( 'NONE',  ( -19.19641293061497223, 270.4323905683720000, -14.20200298773971603 ) ) ;
#1871 = CARTESIAN_POINT ( 'NONE',  ( -36.33955658999052218, 439.1198905601784759, 18.47759065022572500 ) ) ;
#1872 = CARTESIAN_POINT ( 'NONE',  ( -44.16309181155857289, 425.9948905683720568, 6.410867750099241924 ) ) ;
#1873 = CARTESIAN_POINT ( 'NONE',  ( -32.29827456146021092, 51.03054495308385441, 120.7560062544352775 ) ) ;
#1874 = DIRECTION ( 'NONE',  ( -0.000000000000000000, -0.000000000000000000, -1.000000000000000000 ) ) ;
#1875 = DIRECTION ( 'NONE',  ( -0.1238475123623134638, 0.9177839099959486102, 0.3772724323803887114 ) ) ;
#1876 = UNCERTAINTY_MEASURE_WITH_UNIT (LENGTH_MEASURE( 1.000000000000000082E-05 ), #11259, 'distance_accuracy_value', 'NONE');
#1877 = CARTESIAN_POINT ( 'NONE',  ( 60.03793209889851568, 30.52886280891152282, -131.1729372809869005 ) ) ;
#1878 = AXIS2_PLACEMENT_3D ( 'NONE', #20409, #18665, #3544 ) ;
#1879 = CARTESIAN_POINT ( 'NONE',  ( -35.09675569278793716, 323.4948905683720000, -15.47720386886985544 ) ) ;
#1880 = CARTESIAN_POINT ( 'NONE',  ( -11.93348319268873503, 478.5573905683721136, 3.332260488124728415 ) ) ;
#1881 = VERTEX_POINT ( 'NONE', #2974 ) ;
#1882 = CARTESIAN_POINT ( 'NONE',  ( -8.685887942688738761, 491.9323905601785327, 3.978247347593161010 ) ) ;
#1883 = CARTESIAN_POINT ( 'NONE',  ( -38.17536295476244845, 302.3073905683720568, -14.20200298773971426 ) ) ;
#1884 = VECTOR ( 'NONE', #12539, 1000.000000000000000 ) ;
#1885 = CARTESIAN_POINT ( 'NONE',  ( -11.73070664223724613, 341.3073905601785327, 11.32908994701042005 ) ) ;
#1886 = ORIENTED_EDGE ( 'NONE', *, *, #15142, .T. ) ;
#1887 = FACE_BOUND ( 'NONE', #2376, .T. ) ;
#1888 = SHAPE_REPRESENTATION ( 'MAS-323', ( #10032, #3129, #5885, #4845, #16956, #19350, #10019, #7606, #10367, #4175, #3144, #13851, #12473, #13515, #19366, #2813 ), #19031 ) ;
#1889 = CARTESIAN_POINT ( 'NONE',  ( -16.84014894278199392, 409.1198905683720000, 11.84573899990672530 ) ) ;
#1890 = CARTESIAN_POINT ( 'NONE',  ( -45.64106924314018698, 442.9323905765656377, 11.32908994701042538 ) ) ;
#1891 = CARTESIAN_POINT ( 'NONE',  ( -42.82802356641965957, 383.2448905765656377, 14.14213562373094923 ) ) ;
#1892 = CARTESIAN_POINT ( 'NONE',  ( -13.20868407381886911, 429.4948905683720568, -6.410867750099233042 ) ) ;
#1893 = CARTESIAN_POINT ( 'NONE',  ( -42.88789093042841927, 264.4323905683720568, -9.489475012073736337 ) ) ;
#1894 = CARTESIAN_POINT ( 'NONE',  ( -13.20868407381886733, 428.2448905683720568, 6.410867750099229490 ) ) ;
#1895 = SHAPE_DEFINITION_REPRESENTATION ( #6296, #10694 ) ;
#1896 = CARTESIAN_POINT ( 'NONE',  ( 18.55315245287936321, 326.0737056351150613, 25.00000000000000000 ) ) ;
#1897 = CARTESIAN_POINT ( 'NONE',  ( -40.01497788969913927, 360.4323905765656946, -16.95518130045146421 ) ) ;
#1898 = PLANE ( 'NONE',  #3083 ) ;
#1899 = FACE_OUTER_BOUND ( 'NONE', #16616, .T. ) ;
#1900 = CARTESIAN_POINT ( 'NONE',  ( -40.53162694259543741, 332.6198905683720000, -11.84573899990672707 ) ) ;
#1901 = CARTESIAN_POINT ( 'NONE',  ( -11.73070664223726567, 487.9323905765656377, -11.32908994701042538 ) ) ;
#1902 = CIRCLE ( 'NONE', #15023, 125.0000000000000000 ) ;
#1903 = CARTESIAN_POINT ( 'NONE',  ( -19.19641293061499354, 488.8073905683720568, 14.20200298773971426 ) ) ;
#1904 = LINE ( 'NONE', #3080, #947 ) ;
#1905 = DIRECTION ( 'NONE',  ( 1.000000000000000000, 0.000000000000000000, 0.000000000000000000 ) ) ;
#1906 = CARTESIAN_POINT ( 'NONE',  ( -43.68320130047528238, 210.1357463702879613, 0.3279153920022773727 ) ) ;
#1907 = ADVANCED_FACE ( 'NONE', ( #9552 ), #17880, .F. ) ;
#1908 = CARTESIAN_POINT ( 'NONE',  ( -16.84014894278199037, 399.1198905683720000, 11.84573899990672530 ) ) ;
#1909 = CARTESIAN_POINT ( 'NONE',  ( -40.01497788969915348, 470.4323905765656377, -16.95518130045146421 ) ) ;
#1910 = CARTESIAN_POINT ( 'NONE',  ( -45.43829269268869098, 235.0573905683720568, -3.332260488124726194 ) ) ;
#1911 = CARTESIAN_POINT ( 'NONE',  ( -16.84014894278199037, 360.1198905683720000, -11.84573899990672707 ) ) ;
#1912 = VERTEX_POINT ( 'NONE', #6308 ) ;
#1913 = CARTESIAN_POINT ( 'NONE',  ( -35.09675569278797269, 515.7448905683720568, 15.47720386886985366 ) ) ;
#1914 = ORIENTED_EDGE ( 'NONE', *, *, #2617, .T. ) ;
#1915 = CARTESIAN_POINT ( 'NONE',  ( -28.68588794268872277, 437.8698905683720568, 16.75240474999999307 ) ) ;
#1916 = CARTESIAN_POINT ( 'NONE',  ( -40.53162694259545873, 515.1198905683720568, 11.84573899990672885 ) ) ;
#1917 = ORIENTED_EDGE ( 'NONE', *, *, #1923, .T. ) ;
#1918 = DIRECTION ( 'NONE',  ( 0.000000000000000000, 0.000000000000000000, -1.000000000000000000 ) ) ;
#1919 = CARTESIAN_POINT ( 'NONE',  ( -45.43829269268872650, 483.8698905683720568, 0.000000000000000000 ) ) ;
#1920 = VERTEX_POINT ( 'NONE', #12920 ) ;
#1921 = CARTESIAN_POINT ( 'NONE',  ( -25.35362745456399836, 506.6823905683720568, 16.75240474999998952 ) ) ;
#1922 = CARTESIAN_POINT ( 'NONE',  ( -26.10681151960807611, 45.95627095229274772, -49.53444519767779752 ) ) ;
#1923 = EDGE_CURVE ( 'NONE', #3984, #5712, #20048, .T. ) ;
#1924 = CARTESIAN_POINT ( 'NONE',  ( -8.685887942688729879, 426.9948905765656377, -2.449293598294705724E-15 ) ) ;
#1925 = FACE_OUTER_BOUND ( 'NONE', #4549, .T. ) ;
#1926 = CARTESIAN_POINT ( 'NONE',  ( 6.416697501590670427, 172.9933428177121471, -45.00000000000000000 ) ) ;
#1927 = CARTESIAN_POINT ( 'NONE',  ( -48.68588794268871567, 441.9948905765656377, 0.000000000000000000 ) ) ;
#1928 = DIRECTION ( 'NONE',  ( 0.000000000000000000, 0.000000000000000000, -1.000000000000000000 ) ) ;
#1929 = DIRECTION ( 'NONE',  ( -1.191790137725560488E-16, 1.000000000000000000, 0.000000000000000000 ) ) ;
#1930 = SURFACE_STYLE_USAGE ( .BOTH. , #6660 ) ;
#1931 = CARTESIAN_POINT ( 'NONE',  ( -42.91921849944091605, 203.5275734399367025, -4.734433616062221795 ) ) ;
#1932 = CARTESIAN_POINT ( 'NONE',  ( -40.53162694259543031, 306.6198905683720000, 11.84573899990672885 ) ) ;
#1933 = EDGE_CURVE ( 'NONE', #18296, #313, #17169, .T. ) ;
#1934 = CARTESIAN_POINT ( 'NONE',  ( 0.000000000000000000, 0.000000000000000000, 6.500000000000000888 ) ) ;
#1935 = CARTESIAN_POINT ( 'NONE',  ( -40.01497788969912506, 265.6823905601784759, -16.95518130045146421 ) ) ;
#1936 = CARTESIAN_POINT ( 'NONE',  ( -8.685887942688818697, 416.6823905765656377, 3.978247347593374172 ) ) ;
#1937 = CARTESIAN_POINT ( 'NONE',  ( -38.17536295476244135, 296.9323905683720000, 14.20200298773971781 ) ) ;
#1938 = ORIENTED_EDGE ( 'NONE', *, *, #19532, .F. ) ;
#1939 = CARTESIAN_POINT ( 'NONE',  ( -11.73070664223723547, 271.3073905601784759, 11.32908994701042005 ) ) ;
#1940 = CARTESIAN_POINT ( 'NONE',  ( -40.53162694259545873, 506.6198905683721136, 11.84573899990672885 ) ) ;
#1941 = ORIENTED_EDGE ( 'NONE', *, *, #14730, .T. ) ;
#1942 = CARTESIAN_POINT ( 'NONE',  ( -11.93348319268873325, 460.0573905683720568, 3.332260488124728415 ) ) ;
#1943 = CARTESIAN_POINT ( 'NONE',  ( -14.54375231895777532, 408.2448905765655809, -14.14213562373094746 ) ) ;
#1944 = CARTESIAN_POINT ( 'NONE',  ( -19.19641293061497578, 270.4323905683720000, -14.20200298773971603 ) ) ;
#1945 = EDGE_LOOP ( 'NONE', ( #2595, #4010, #7835, #17534 ) ) ;
#1946 = CARTESIAN_POINT ( 'NONE',  ( -40.01497788969913216, 333.5573905765655809, 16.95518130045146776 ) ) ;
#1947 = CARTESIAN_POINT ( 'NONE',  ( -25.35362745456398059, 272.5573905683720568, -16.75240474999999307 ) ) ;
#1948 = CARTESIAN_POINT ( 'NONE',  ( -40.53162694259542320, 246.6198905683720284, 11.84573899990672885 ) ) ;
#1949 = CARTESIAN_POINT ( 'NONE',  ( -47.16347859291443001, 251.3698905765656093, -7.653668647301793193 ) ) ;
#1950 = CARTESIAN_POINT ( 'NONE',  ( -48.68588794268871567, 421.9948905765656377, 0.000000000000000000 ) ) ;
#1951 = CARTESIAN_POINT ( 'NONE',  ( -48.68588794268869435, 227.2448905601785043, 0.000000000000000000 ) ) ;
#1952 = CARTESIAN_POINT ( 'NONE',  ( -14.48388495494898542, 257.9323905683720568, 9.489475012073732785 ) ) ;
#1953 = CARTESIAN_POINT ( 'NONE',  ( -16.84014894278198682, 349.1198905683720568, 11.84573899990672530 ) ) ;
#1954 = CARTESIAN_POINT ( 'NONE',  ( -24.70764059509557597, 504.4323905601785327, -19.99999999999999289 ) ) ;
#1955 = B_SPLINE_CURVE_WITH_KNOTS ( 'NONE', 3,
 ( #15011, #11532, #8271, #13051, #5037, #19970 ),
 .UNSPECIFIED., .F., .F.,
 ( 4, 2, 4 ),
 ( 0.006874058788776910706, 0.008773169699270545047, 0.01067228060976418112 ),
 .UNSPECIFIED. ) ;
#1956 = CARTESIAN_POINT ( 'NONE',  ( -35.09675569278795848, 395.7448905683720568, 15.47720386886985366 ) ) ;
#1957 = DIRECTION ( 'NONE',  ( 0.000000000000000000, 1.000000000000000000, 0.000000000000000000 ) ) ;
#1958 = ORIENTED_EDGE ( 'NONE', *, *, #1583, .F. ) ;
#1959 = CARTESIAN_POINT ( 'NONE',  ( -48.68588794268871567, 397.5573905601785327, 3.978247347593168115 ) ) ;
#1960 = ORIENTED_EDGE ( 'NONE', *, *, #10517, .T. ) ;
#1961 = ORIENTED_EDGE ( 'NONE', *, *, #2820, .F. ) ;
#1962 = ORIENTED_EDGE ( 'NONE', *, *, #18558, .T. ) ;
#1963 = CARTESIAN_POINT ( 'NONE',  ( -40.53162694259545873, 526.6198905683720568, 11.84573899990672885 ) ) ;
#1964 = CARTESIAN_POINT ( 'NONE',  ( -40.01497788969913216, 295.6823905601784190, -16.95518130045146421 ) ) ;
#1965 = DIRECTION ( 'NONE',  ( 0.000000000000000000, 0.000000000000000000, -1.000000000000000000 ) ) ;
#1966 = ADVANCED_FACE ( 'NONE', ( #5225 ), #13352, .F. ) ;
#1967 = CARTESIAN_POINT ( 'NONE',  ( -22.27502019258947286, 318.4948905683720000, 15.47720386886985189 ) ) ;
#1968 = CARTESIAN_POINT ( 'NONE',  ( -28.68588794268871567, 361.3698905683720568, -16.75240474999999307 ) ) ;
#1969 = EDGE_CURVE ( 'NONE', #629, #9649, #273, .T. ) ;
#1970 = CARTESIAN_POINT ( 'NONE',  ( -45.43829269268871229, 373.5573905683720568, -3.332260488124726638 ) ) ;
#1971 = EDGE_CURVE ( 'NONE', #8699, #13316, #1399, .T. ) ;
#1972 = VECTOR ( 'NONE', #15412, 1000.000000000000114 ) ;
#1973 = CARTESIAN_POINT ( 'NONE',  ( -17.35679799567828496, 295.4323905765655809, 16.95518130045146421 ) ) ;
#1974 = CARTESIAN_POINT ( 'NONE',  ( -31.26501780185373391, 205.1437886375728965, 0.000000000000000000 ) ) ;
#1975 = CARTESIAN_POINT ( 'NONE',  ( -13.20868407381884779, 258.2448905683720000, 6.410867750099229490 ) ) ;
#1976 = DIRECTION ( 'NONE',  ( -1.191790137725560488E-16, 1.000000000000000000, -0.000000000000000000 ) ) ;
#1977 = CARTESIAN_POINT ( 'NONE',  ( -28.68588794268871922, 417.8698905683720568, 16.75240474999999307 ) ) ;
#1978 = VECTOR ( 'NONE', #2773, 1000.000000000000000 ) ;
#1979 = DIRECTION ( 'NONE',  ( 1.191790137725560488E-16, -1.000000000000000000, -0.000000000000000000 ) ) ;
#1980 = CARTESIAN_POINT ( 'NONE',  ( -8.685887942688724550, 382.2448905601784759, -2.449293598294705724E-15 ) ) ;
#1981 = CARTESIAN_POINT ( 'NONE',  ( 146.1533239063698772, 585.7448905601785327, 7.500000000000000000 ) ) ;
#1982 = EDGE_CURVE ( 'NONE', #1165, #11758, #16256, .T. ) ;
#1983 = CARTESIAN_POINT ( 'NONE',  ( -32.01814843081344719, 337.5573905683720000, 16.75240474999999307 ) ) ;
#1984 = CARTESIAN_POINT ( 'NONE',  ( -45.43829269268871940, 464.1823905683720568, 3.332260488124734632 ) ) ;
#1985 = ORIENTED_EDGE ( 'NONE', *, *, #3021, .F. ) ;
#1986 = CARTESIAN_POINT ( 'NONE',  ( -28.68588794268872988, 474.7448905601784759, -19.99999999999999289 ) ) ;
#1987 = CARTESIAN_POINT ( 'NONE',  ( -11.93348319268871549, 298.5573905683720000, 3.332260488124728415 ) ) ;
#1988 = AXIS2_PLACEMENT_3D ( 'NONE', #4495, #15868, #2663 ) ;
#1989 = CARTESIAN_POINT ( 'NONE',  ( -32.66413529028186957, 344.1823905765656377, 19.99999999999999289 ) ) ;
#1990 = EDGE_LOOP ( 'NONE', ( #11807, #14723, #7245, #9725, #847, #446, #5765, #1066, #1635, #898, #9045, #9093, #16986, #2971, #7661, #12828, #15871, #17451, #18057, #7387, #6965, #3861, #3418, #2324, #9228, #8611 ) ) ;
#1991 = FACE_OUTER_BOUND ( 'NONE', #18934, .T. ) ;
#1992 = CARTESIAN_POINT ( 'NONE',  ( -14.54375231895776821, 343.4948905601785327, -14.14213562373094746 ) ) ;
#1993 =( REPRESENTATION_RELATIONSHIP ('NONE','NONE', #1888, #4206 ) REPRESENTATION_RELATIONSHIP_WITH_TRANSFORMATION ( #909 )SHAPE_REPRESENTATION_RELATIONSHIP( ) );
#1994 = AXIS2_PLACEMENT_3D ( 'NONE', #16072, #16178, #18981 ) ;
#1995 = CARTESIAN_POINT ( 'NONE',  ( -11.93348319268872260, 380.6823905683720568, -3.332260488124732856 ) ) ;
#1996 = CARTESIAN_POINT ( 'NONE',  ( 4.700000000000000178, 0.000000000000000000, 0.000000000000000000 ) ) ;
#1997 = CARTESIAN_POINT ( 'NONE',  ( -45.43829269268871229, 423.5573905683720000, -3.332260488124726194 ) ) ;
#1998 = CARTESIAN_POINT ( 'NONE',  ( -19.19641293061496867, 258.8073905683720000, 14.20200298773971426 ) ) ;
#1999 = CARTESIAN_POINT ( 'NONE',  ( -22.27502019258948351, 426.9948905683720568, 15.47720386886985189 ) ) ;
#2000 = APPLICATION_PROTOCOL_DEFINITION ( 'draft international standard', 'automotive_design', 1998, #887 ) ;
#2001 = DIRECTION ( 'NONE',  ( 0.000000000000000000, -1.000000000000000000, 0.000000000000000000 ) ) ;
#2002 = CARTESIAN_POINT ( 'NONE',  ( -42.82802356641965957, 363.2448905765656377, 14.14213562373094923 ) ) ;
#2003 = CYLINDRICAL_SURFACE ( 'NONE', #20003, 5.000000000000004441 ) ;
#2004 = LINE ( 'NONE', #380, #19948 ) ;
#2005 = CARTESIAN_POINT ( 'NONE',  ( -13.20868407381885667, 329.4948905683720568, -6.410867750099233042 ) ) ;
#2006 = DIRECTION ( 'NONE',  ( -0.000000000000000000, -0.000000000000000000, 1.000000000000000000 ) ) ;
#2007 = CARTESIAN_POINT ( 'NONE',  ( -32.01814843081346140, 483.1823905683720000, -16.75240474999999307 ) ) ;
#2008 = VECTOR ( 'NONE', #1202, 1000.000000000000000 ) ;
#2009 = CARTESIAN_POINT ( 'NONE',  ( -8.685887942688729879, 442.2448905601785327, -2.449293598294705724E-15 ) ) ;
#2010 = CARTESIAN_POINT ( 'NONE',  ( -21.03221929538691626, 304.1198905601785327, -18.47759065022572855 ) ) ;
#2011 = CIRCLE ( 'NONE', #4057, 40.00000000000000000 ) ;
#2012 = CARTESIAN_POINT ( 'NONE',  ( -35.09675569278795138, 393.4948905683720000, -15.47720386886985544 ) ) ;
#2013 = CARTESIAN_POINT ( 'NONE',  ( -48.68588794268872277, 471.9948905765656377, 0.000000000000000000 ) ) ;
#2014 = CARTESIAN_POINT ( 'NONE',  ( -36.33955658999052929, 525.3698905601784190, -18.47759065022572855 ) ) ;
#2015 = CARTESIAN_POINT ( 'NONE',  ( -25.35362745456398059, 366.6823905683720000, 16.75240474999998952 ) ) ;
#2016 = EDGE_LOOP ( 'NONE', ( #12187, #20247 ) ) ;
#2017 = CARTESIAN_POINT ( 'NONE',  ( -19.19641293061500065, 527.3073905683720568, 14.20200298773971426 ) ) ;
#2018 = ORIENTED_EDGE ( 'NONE', *, *, #9858, .T. ) ;
#2019 = CARTESIAN_POINT ( 'NONE',  ( -11.93348319268874036, 518.5573905683720568, 3.332260488124728415 ) ) ;
#2020 = ORIENTED_EDGE ( 'NONE', *, *, #19133, .T. ) ;
#2021 = CARTESIAN_POINT ( 'NONE',  ( -42.82802356641964536, 205.1437886375728965, 5.000000000000001776 ) ) ;
#2022 = CARTESIAN_POINT ( 'NONE',  ( -11.93348319268873503, 479.1823905683721136, -3.332260488124732856 ) ) ;
#2023 = ORIENTED_EDGE ( 'NONE', *, *, #10335, .T. ) ;
#2024 = CARTESIAN_POINT ( 'NONE',  ( -11.93348319268873681, 488.5573905683720568, 3.332260488124728859 ) ) ;
#2025 = CARTESIAN_POINT ( 'NONE',  ( -8.685887942688736985, 492.2448905601785327, -2.449293598294705724E-15 ) ) ;
#2026 = ADVANCED_FACE ( 'NONE', ( #3292 ), #3499, .T. ) ;
#2027 = CARTESIAN_POINT ( 'NONE',  ( -45.64106924314019409, 421.0573905765655809, -11.32908994701042715 ) ) ;
#2028 = CARTESIAN_POINT ( 'NONE',  ( -28.68588794268872633, 250.8848358243226357, 0.000000000000000000 ) ) ;
#2029 = CARTESIAN_POINT ( 'NONE',  ( -28.68588794268872633, 439.4948905765655809, -19.99999999999999289 ) ) ;
#2030 = DIRECTION ( 'NONE',  ( -0.000000000000000000, -1.000000000000000000, -0.000000000000000000 ) ) ;
#2031 = FACE_OUTER_BOUND ( 'NONE', #11176, .T. ) ;
#2032 = CARTESIAN_POINT ( 'NONE',  ( -21.03221929538692692, 495.1198905765656377, 18.47759065022572500 ) ) ;
#2033 = CARTESIAN_POINT ( 'NONE',  ( -32.01814843081344009, 303.1823905683720000, -16.75240474999999307 ) ) ;
#2034 = FACE_OUTER_BOUND ( 'NONE', #10469, .T. ) ;
#2035 = CARTESIAN_POINT ( 'NONE',  ( -14.48388495494900674, 449.4323905683720568, 9.489475012073732785 ) ) ;
#2036 = CARTESIAN_POINT ( 'NONE',  ( -28.68588794268872633, 333.8848358243226357, -20.00000000000000000 ) ) ;
#2037 = ORIENTED_EDGE ( 'NONE', *, *, #21318, .T. ) ;
#2038 = CARTESIAN_POINT ( 'NONE',  ( -48.68588794268872988, 536.9323905601785327, -3.978247347593157901 ) ) ;
#2039 = CARTESIAN_POINT ( 'NONE',  ( -25.35362745456399836, 498.1823905683720568, 16.75240474999998952 ) ) ;
#2040 = ORIENTED_EDGE ( 'NONE', *, *, #13784, .T. ) ;
#2041 = CARTESIAN_POINT ( 'NONE',  ( -45.43829269268871940, 465.0573905683720000, -3.332260488124726194 ) ) ;
#2042 = LINE ( 'NONE', #17070, #4161 ) ;
#2043 = CARTESIAN_POINT ( 'NONE',  ( -28.68588794268870146, 266.3698905683720000, 16.75240474999999307 ) ) ;
#2044 = ORIENTED_EDGE ( 'NONE', *, *, #7088, .T. ) ;
#2045 = CARTESIAN_POINT ( 'NONE',  ( -8.685887942688898633, 336.6823905765656377, 3.978247347593586447 ) ) ;
#2046 = EDGE_CURVE ( 'NONE', #12320, #10687, #11847, .T. ) ;
#2047 = CARTESIAN_POINT ( 'NONE',  ( -24.70764059509555111, 309.1823905765656377, -19.99999999999999289 ) ) ;
#2048 = CARTESIAN_POINT ( 'NONE',  ( -19.19641293061496512, 238.8073905683720284, 14.20200298773971426 ) ) ;
#2049 = CARTESIAN_POINT ( 'NONE',  ( -32.66413529028186247, 309.4323905601785327, 19.99999999999999289 ) ) ;
#2050 = FACE_OUTER_BOUND ( 'NONE', #14540, .T. ) ;
#2051 = CARTESIAN_POINT ( 'NONE',  ( -42.88789093042841927, 262.9323905683720568, -9.489475012073736337 ) ) ;
#2052 = CARTESIAN_POINT ( 'NONE',  ( -42.88789093042843348, 366.3073905683720000, 9.489475012073736337 ) ) ;
#2053 = CARTESIAN_POINT ( 'NONE',  ( -42.82802356641965247, 278.4948905601785327, 14.14213562373094923 ) ) ;
#2054 = AXIS2_PLACEMENT_3D ( 'NONE', #10858, #1148, #7719 ) ;
#2055 = EDGE_CURVE ( 'NONE', #10338, #15635, #16707, .T. ) ;
#2056 = CARTESIAN_POINT ( 'NONE',  ( -28.68588794268871922, 406.3698905683720000, 16.75240474999999307 ) ) ;
#2057 = CARTESIAN_POINT ( 'NONE',  ( -47.16347859291445843, 507.8698905601785327, 7.653668647301805628 ) ) ;
#2058 = CARTESIAN_POINT ( 'NONE',  ( -32.66413529028188378, 399.4323905601784759, 19.99999999999999289 ) ) ;
#2059 = EDGE_LOOP ( 'NONE', ( #17770, #21021, #12429, #7123 ) ) ;
#2060 = ORIENTED_EDGE ( 'NONE', *, *, #8116, .F. ) ;
#2061 = ORIENTED_EDGE ( 'NONE', *, *, #13941, .T. ) ;
#2062 = CARTESIAN_POINT ( 'NONE',  ( -14.48388495494901740, 521.3073905683720568, -9.489475012073736337 ) ) ;
#2063 = VECTOR ( 'NONE', #19720, 1000.000000000000000 ) ;
#2064 = CARTESIAN_POINT ( 'NONE',  ( -8.685887942688712116, 282.2448905601784759, -2.449293598294705724E-15 ) ) ;
#2065 = DIRECTION ( 'NONE',  ( -0.000000000000000000, -0.000000000000000000, -1.000000000000000000 ) ) ;
#2066 = CARTESIAN_POINT ( 'NONE',  ( -38.17536295476244135, 316.9323905683719431, 14.20200298773971781 ) ) ;
#2067 = EDGE_LOOP ( 'NONE', ( #9854, #18586 ) ) ;
#2068 = CARTESIAN_POINT ( 'NONE',  ( -35.09675569278795138, 365.7448905683720568, 15.47720386886985366 ) ) ;
#2069 = CARTESIAN_POINT ( 'NONE',  ( -13.20868407381886200, 369.4948905683720568, -6.410867750099233042 ) ) ;
#2070 = CARTESIAN_POINT ( 'NONE',  ( -8.685887942688717445, 306.9948905765655809, -2.449293598294705724E-15 ) ) ;
#2071 = DIRECTION ( 'NONE',  ( -0.000000000000000000, -0.000000000000000000, -1.000000000000000000 ) ) ;
#2072 = CARTESIAN_POINT ( 'NONE',  ( -25.35362745456396638, 256.6823905683720000, 16.75240474999998952 ) ) ;
#2073 = CARTESIAN_POINT ( 'NONE',  ( -43.67482055103364047, 200.1767183643994770, 0.6599055232175832231 ) ) ;
#2074 = CARTESIAN_POINT ( 'NONE',  ( -40.53162694259544452, 426.6198905683720000, 11.84573899990672885 ) ) ;
#2075 = CARTESIAN_POINT ( 'NONE',  ( -165.7253922195053519, 600.7448905601785327, -108.8355377051282034 ) ) ;
#2076 = CARTESIAN_POINT ( 'NONE',  ( -48.68588794268861619, 356.9323905601784190, -3.978247347593371508 ) ) ;
#2077 = CARTESIAN_POINT ( 'NONE',  ( -42.82802356641965247, 273.2448905765656377, 14.14213562373094923 ) ) ;
#2078 = PRODUCT_DEFINITION_CONTEXT ( 'detailed design', #15254, 'design' ) ;
#2079 = CARTESIAN_POINT ( 'NONE',  ( -10.20829729246299067, 411.6198905601784759, 7.653668647301790529 ) ) ;
#2080 = CARTESIAN_POINT ( 'NONE',  ( -44.16309181155856578, 335.9948905683720000, 6.410867750099241924 ) ) ;
#2081 = CARTESIAN_POINT ( 'NONE',  ( -13.20868407381887444, 469.4948905683720000, -6.410867750099233042 ) ) ;
#2082 = VERTEX_POINT ( 'NONE', #11927 ) ;
#2083 = CARTESIAN_POINT ( 'NONE',  ( -14.54375231895778242, 463.4948905601785327, -14.14213562373094746 ) ) ;
#2084 = CARTESIAN_POINT ( 'NONE',  ( -42.88789093042842637, 282.9323905683721136, -9.489475012073736337 ) ) ;
#2085 = CARTESIAN_POINT ( 'NONE',  ( -14.54375231895776466, 340.9948905601784759, 14.14213562373094568 ) ) ;
#2086 = VERTEX_POINT ( 'NONE', #5010 ) ;
#2087 = LINE ( 'NONE', #16698, #11544 ) ;
#2088 = CARTESIAN_POINT ( 'NONE',  ( -14.54375231895776466, 340.9948905601784759, 14.14213562373094568 ) ) ;
#2089 = CARTESIAN_POINT ( 'NONE',  ( -32.01814843081344719, 393.1823905683721136, -16.75240474999999307 ) ) ;
#2090 = CARTESIAN_POINT ( 'NONE',  ( -11.73070664223723014, 231.3073905601784475, 11.32908994701042005 ) ) ;
#2091 = CARTESIAN_POINT ( 'NONE',  ( -28.68588794268874054, 573.2448905601785327, 0.000000000000000000 ) ) ;
#2092 = CARTESIAN_POINT ( 'NONE',  ( -32.01814843081345430, 421.6823905683720568, -16.75240474999999307 ) ) ;
#2093 = CARTESIAN_POINT ( 'NONE',  ( -19.19641293061497578, 261.9323905683720568, -14.20200298773971603 ) ) ;
#2094 = VECTOR ( 'NONE', #11631, 1000.000000000000114 ) ;
#2095 = EDGE_CURVE ( 'NONE', #11573, #6399, #18201, .T. ) ;
#2096 = CARTESIAN_POINT ( 'NONE',  ( -44.16309181155857999, 433.2448905683720000, -6.410867750099231266 ) ) ;
#2097 = APPLICATION_PROTOCOL_DEFINITION ( 'draft international standard', 'automotive_design', 1998, #7359 ) ;
#2098 = EDGE_CURVE ( 'NONE', #2934, #3515, #9978, .T. ) ;
#2099 = CARTESIAN_POINT ( 'NONE',  ( -47.16347859291444422, 362.6198905765656377, 7.653668647301805628 ) ) ;
#2100 = CARTESIAN_POINT ( 'NONE',  ( -14.54375231895775933, 273.4948905601785327, -14.14213562373094746 ) ) ;
#2101 = CARTESIAN_POINT ( 'NONE',  ( -14.48388495494899431, 319.8073905683720568, -9.489475012073734561 ) ) ;
#2102 = LINE ( 'NONE', #18423, #9341 ) ;
#2103 = CARTESIAN_POINT ( 'NONE',  ( -25.35362745456399480, 478.1823905683720568, 16.75240474999998952 ) ) ;
#2105 = DIRECTION ( 'NONE',  ( 0.000000000000000000, -0.5000000000000009992, 0.8660254037844381525 ) ) ;
#2104 = AXIS2_PLACEMENT_3D ( 'NONE', #6741, #278, #7476 ) ;
#2106 = CARTESIAN_POINT ( 'NONE',  ( -43.31864445205426506, 201.3798797254112571, -3.307266650052995249 ) ) ;
#2107 = CARTESIAN_POINT ( 'NONE',  ( -21.03221929538689494, 225.1198905765656093, 18.47759065022572500 ) ) ;
#2108 = VECTOR ( 'NONE', #6888, 1000.000000000000000 ) ;
#2109 = CARTESIAN_POINT ( 'NONE',  ( -16.84014894278199037, 389.1198905683720568, 11.84573899990672530 ) ) ;
#2110 = CIRCLE ( 'NONE', #3489, 20.00000000000000000 ) ;
#2111 = CARTESIAN_POINT ( 'NONE',  ( -30.95961475400111240, 49.18261979607746071, -121.1065849196700128 ) ) ;
#2112 = CARTESIAN_POINT ( 'NONE',  ( -8.685887942688742314, 522.5573905601785327, -3.978247347593165895 ) ) ;
#2113 = CARTESIAN_POINT ( 'NONE',  ( -38.17536295476244845, 355.4323905683720568, 14.20200298773971781 ) ) ;
#2114 = ORIENTED_EDGE ( 'NONE', *, *, #3555, .T. ) ;
#2115 = CARTESIAN_POINT ( 'NONE',  ( -44.16309181155858710, 524.4948905683719431, 6.410867750099241924 ) ) ;
#2116 = VERTEX_POINT ( 'NONE', #1788 ) ;
#2117 = CARTESIAN_POINT ( 'NONE',  ( -17.35679799567829917, 353.8073905601784759, -16.95518130045146421 ) ) ;
#2118 = CARTESIAN_POINT ( 'NONE',  ( -45.43829269268872650, 514.1823905683719431, 3.332260488124734632 ) ) ;
#2119 = VERTEX_POINT ( 'NONE', #6736 ) ;
#2120 = CARTESIAN_POINT ( 'NONE',  ( -32.01814843081346140, 476.0573905683720000, 16.75240474999999307 ) ) ;
#2121 = VERTEX_POINT ( 'NONE', #8355 ) ;
#2122 = CARTESIAN_POINT ( 'NONE',  ( -45.43829269268872650, 483.5573905683720000, -3.332260488124726638 ) ) ;
#2123 = CARTESIAN_POINT ( 'NONE',  ( -24.70764059509556176, 490.0573905601784190, 19.99999999999998934 ) ) ;
#2125 = AXIS2_PLACEMENT_3D ( 'NONE', #18739, #699, #7268 ) ;
#2124 = CARTESIAN_POINT ( 'NONE',  ( -8.685887942688728103, 416.6823905765656377, 3.978247347593161010 ) ) ;
#2126 = LINE ( 'NONE', #514, #8599 ) ;
#2127 = CARTESIAN_POINT ( 'NONE',  ( -8.685887942688980345, 301.9323905601784190, 3.978247347593800054 ) ) ;
#2128 = CARTESIAN_POINT ( 'NONE',  ( -48.68588794268873698, 573.2448905601785327, 0.000000000000000000 ) ) ;
#2129 = CARTESIAN_POINT ( 'NONE',  ( -28.68588794268873698, 548.2448905601784190, 0.000000000000000000 ) ) ;
#2130 = CARTESIAN_POINT ( 'NONE',  ( 18.20947592957834260, 600.7448905601785327, -168.5995991907681173 ) ) ;
#2131 =( BOUNDED_CURVE ( )  B_SPLINE_CURVE ( 2, ( #17586, #8930, #12188, #18992, #5904, #9364, #19108, #2458, #15872, #15555, #15979, #14037, #17380, #2561, #9038, #15764, #17479 ),
 .UNSPECIFIED., .F., .T. ) 
 B_SPLINE_CURVE_WITH_KNOTS ( ( 3, 2, 2, 2, 2, 2, 2, 2, 3 ),
 ( 0.1562500000000001388, 0.1582031250000001388, 0.1601562500000001388, 0.1621093750000001388, 0.1640625000000001665, 0.1660156250000001665, 0.1679687500000001665, 0.1699218750000001665, 0.1718750000000001665 ),
 .UNSPECIFIED. ) 
 CURVE ( )  GEOMETRIC_REPRESENTATION_ITEM ( )  RATIONAL_B_SPLINE_CURVE ( ( 0.9999999999999986677, 0.9807852804032317628, 1.000000000000000000, 0.9807852804032304306, 1.000000000000000000, 0.9807852804032304306, 1.000000000000000000, 0.9807852804032304306, 1.000000000000000000, 0.9807852804032304306, 1.000000000000000000, 0.9807852804032304306, 1.000000000000000000, 0.9807852804032304306, 1.000000000000000000, 0.9807852804032287652, 1.000000000000001554 ) ) 
 REPRESENTATION_ITEM ( '' )  );
#2132 = CARTESIAN_POINT ( 'NONE',  ( -13.20868407381885312, 300.9948905683720568, -6.410867750099233042 ) ) ;
#2133 = CARTESIAN_POINT ( 'NONE',  ( 158.8141120573112630, 10.52886280891152104, 0.000000000000000000 ) ) ;
#2134 = CARTESIAN_POINT ( 'NONE',  ( -35.09675569278795848, 447.2448905683720000, 15.47720386886985366 ) ) ;
#2135 = LINE ( 'NONE', #2245, #16838 ) ;
#2136 = CARTESIAN_POINT ( 'NONE',  ( -45.43829269268869098, 265.6823905683720568, 3.332260488124734632 ) ) ;
#2137 = VERTEX_POINT ( 'NONE', #19940 ) ;
#2138 = CARTESIAN_POINT ( 'NONE',  ( -47.16347859291443001, 267.8698905601784759, 7.653668647301805628 ) ) ;
#2139 = CARTESIAN_POINT ( 'NONE',  ( -35.09675569278797269, 507.2448905683719431, 15.47720386886985366 ) ) ;
#2140 = EDGE_CURVE ( 'NONE', #3989, #15664, #6840, .T. ) ;
#2141 = ORIENTED_EDGE ( 'NONE', *, *, #11380, .F. ) ;
#2142 = CARTESIAN_POINT ( 'NONE',  ( -14.48388495494901029, 461.3073905683720568, -9.489475012073736337 ) ) ;
#2143 = ADVANCED_FACE ( 'NONE', ( #4751 ), #7988, .F. ) ;
#2144 = DIRECTION ( 'NONE',  ( -1.000000000000000000, 0.000000000000000000, 0.000000000000000000 ) ) ;
#2145 = CARTESIAN_POINT ( 'NONE',  ( -44.16309181155855867, 253.2448905683720284, -6.410867750099231266 ) ) ;
#2146 = ORIENTED_EDGE ( 'NONE', *, *, #8477, .F. ) ;
#2147 = CARTESIAN_POINT ( 'NONE',  ( 91.21585410611801592, 56.85652257517428865, 94.99999999999994316 ) ) ;
#2148 = CARTESIAN_POINT ( 'NONE',  ( -35.09675569278793716, 267.2448905683720568, 15.47720386886985366 ) ) ;
#2149 = CARTESIAN_POINT ( 'NONE',  ( -10.20829729246299955, 477.6198905765656377, -7.653668647301794969 ) ) ;
#2150 = CARTESIAN_POINT ( 'NONE',  ( 146.3141120573112630, 585.7448905601785327, 0.000000000000000000 ) ) ;
#2151 = CARTESIAN_POINT ( 'NONE',  ( -11.93348319268870661, 250.6823905683720568, -3.332260488124732856 ) ) ;
#2152 = CARTESIAN_POINT ( 'NONE',  ( 5.674999999999999822, -3.752776749732576356, -6.500000000000000000 ) ) ;
#2153 = CYLINDRICAL_SURFACE ( 'NONE', #9746, 4.000000000000001776 ) ;
#2154 = CARTESIAN_POINT ( 'NONE',  ( 0.000000000000000000, 0.000000000000000000, 0.000000000000000000 ) ) ;
#2155 = CARTESIAN_POINT ( 'NONE',  ( -19.19641293061497223, 250.4323905683720284, -14.20200298773971603 ) ) ;
#2156 = CIRCLE ( 'NONE', #17007, 4.999999999999990230 ) ;
#2157 = CARTESIAN_POINT ( 'NONE',  ( -42.88789093042843348, 356.3073905683720000, 9.489475012073736337 ) ) ;
#2158 = DIRECTION ( 'NONE',  ( 0.000000000000000000, 0.000000000000000000, -1.000000000000000000 ) ) ;
#2159 = EDGE_CURVE ( 'NONE', #1196, #10794, #11347, .T. ) ;
#2160 = CARTESIAN_POINT ( 'NONE',  ( -42.88789093042844058, 402.9323905683720000, -9.489475012073736337 ) ) ;
#2161 = CARTESIAN_POINT ( 'NONE',  ( -48.68588794268870856, 341.9948905765656377, 0.000000000000000000 ) ) ;
#2162 = CIRCLE ( 'NONE', #7675, 4.000000000000001776 ) ;
#2163 = CARTESIAN_POINT ( 'NONE',  ( -8.685887942688726326, 401.9323905601784190, 3.978247347593161010 ) ) ;
#2164 = EDGE_LOOP ( 'NONE', ( #7943, #957, #5762 ) ) ;
#2165 = CARTESIAN_POINT ( 'NONE',  ( -17.35679799567829562, 348.5573905765655809, -16.95518130045146421 ) ) ;
#2166 = ORIENTED_EDGE ( 'NONE', *, *, #1295, .F. ) ;
#2167 = ORIENTED_EDGE ( 'NONE', *, *, #1499, .F. ) ;
#2168 = CARTESIAN_POINT ( 'NONE',  ( -35.09675569278797269, 527.2448905683719431, 15.47720386886985366 ) ) ;
#2169 = CARTESIAN_POINT ( 'NONE',  ( -32.66413529028186957, 289.4323905601784759, 19.99999999999999289 ) ) ;
#2170 = DIRECTION ( 'NONE',  ( -1.000000000000000000, -0.000000000000000000, -0.000000000000000000 ) ) ;
#2171 = CARTESIAN_POINT ( 'NONE',  ( -42.88789093042842637, 314.4323905683719431, -9.489475012073734561 ) ) ;
#2172 = CARTESIAN_POINT ( 'NONE',  ( -13.20868407381885667, 338.2448905683720568, 6.410867750099229490 ) ) ;
#2173 = CARTESIAN_POINT ( 'NONE',  ( -13.20868407381886023, 368.2448905683720000, 6.410867750099229490 ) ) ;
#2174 = ADVANCED_FACE ( 'NONE', ( #11454 ), #1208, .T. ) ;
#2175 = CARTESIAN_POINT ( 'NONE',  ( -48.68588794268870146, 291.6823905765656377, -3.978247347593158345 ) ) ;
#2176 = DIRECTION ( 'NONE',  ( 1.000000000000000000, 0.000000000000000000, 0.000000000000000000 ) ) ;
#2177 = CARTESIAN_POINT ( 'NONE',  ( -44.16309181155855867, 263.2448905683720000, -6.410867750099231266 ) ) ;
#2178 = LINE ( 'NONE', #8971, #4278 ) ;
#2179 = AXIS2_PLACEMENT_3D ( 'NONE', #15173, #18818, #6926 ) ;
#2180 = CARTESIAN_POINT ( 'NONE',  ( -11.93348319268872615, 410.3698905683720568, -2.051577885510841163E-15 ) ) ;
#2181 = CARTESIAN_POINT ( 'NONE',  ( -25.29117952274775760, 45.70212558035238715, 122.4152406641337478 ) ) ;
#2182 = CARTESIAN_POINT ( 'NONE',  ( -21.03221929538693402, 448.8698905765656377, -18.47759065022572855 ) ) ;
#2183 = CARTESIAN_POINT ( 'NONE',  ( -28.68588794268875120, 585.7448905601785327, 0.000000000000000000 ) ) ;
#2184 = EDGE_CURVE ( 'NONE', #18163, #3421, #21368, .T. ) ;
#2185 = CARTESIAN_POINT ( 'NONE',  ( -11.93348319268871727, 320.6823905683720000, -3.332260488124732856 ) ) ;
#2186 = CARTESIAN_POINT ( 'NONE',  ( -45.43829269268872650, 463.8698905683720000, 0.000000000000000000 ) ) ;
#2187 = EDGE_LOOP ( 'NONE', ( #11092, #20552, #125, #11975 ) ) ;
#2188 = CARTESIAN_POINT ( 'NONE',  ( -36.33955658999052929, 469.1198905601784759, 18.47759065022572500 ) ) ;
#2189 = CARTESIAN_POINT ( 'NONE',  ( -19.19641293061497578, 280.4323905683720568, -14.20200298773971603 ) ) ;
#2190 = AXIS2_PLACEMENT_3D ( 'NONE', #13659, #13235, #5001 ) ;
#2191 = EDGE_LOOP ( 'NONE', ( #4997, #14936, #2251, #12373, #1258, #8230 ) ) ;
#2192 = ORIENTED_EDGE ( 'NONE', *, *, #11921, .F. ) ;
#2193 = CARTESIAN_POINT ( 'NONE',  ( -43.68588794268869435, 188.9102039777116602, 0.000000000000000000 ) ) ;
#2194 = CIRCLE ( 'NONE', #7691, 15.00000000000000355 ) ;
#2195 = CARTESIAN_POINT ( 'NONE',  ( -14.48388495494899253, 299.8073905683720000, -9.489475012073736337 ) ) ;
#2196 = CARTESIAN_POINT ( 'NONE',  ( -22.27502019258947996, 378.4948905683720000, 15.47720386886985189 ) ) ;
#2197 = CARTESIAN_POINT ( 'NONE',  ( -40.01497788969913216, 295.6823905601784190, -16.95518130045146421 ) ) ;
#2198 = CARTESIAN_POINT ( 'NONE',  ( -42.82802356641968089, 520.7448905765656946, -14.14213562373094746 ) ) ;
#2199 = CARTESIAN_POINT ( 'NONE',  ( -40.53162694259544452, 412.6198905683720568, -11.84573899990672707 ) ) ;
#2200 = CARTESIAN_POINT ( 'NONE',  ( -28.68588794268870501, 262.8698905683720000, -16.75240474999999307 ) ) ;
#2201 = CARTESIAN_POINT ( 'NONE',  ( -11.93348319268872970, 429.1823905683720568, -3.332260488124732856 ) ) ;
#2202 = CARTESIAN_POINT ( 'NONE',  ( -45.64106924314018698, 372.9323905765655809, 11.32908994701042715 ) ) ;
#2203 = CARTESIAN_POINT ( 'NONE',  ( 43.53705524234220547, -133.1434774248255906, 96.62835994548002816 ) ) ;
#2204 = CARTESIAN_POINT ( 'NONE',  ( -14.48388495494899253, 317.9323905683719431, 9.489475012073731008 ) ) ;
#2205 = CARTESIAN_POINT ( 'NONE',  ( -35.09675569278795848, 473.4948905683720000, -15.47720386886985544 ) ) ;
#2206 = VECTOR ( 'NONE', #9331, 1000.000000000000000 ) ;
#2207 = CARTESIAN_POINT ( 'NONE',  ( 20.42502041961813930, 230.5765313837437418, -60.00000000000000000 ) ) ;
#2208 = CARTESIAN_POINT ( 'NONE',  ( -43.37470026482863972, 201.1699573972600774, -3.051950158715578176 ) ) ;
#2209 = CARTESIAN_POINT ( 'NONE',  ( 60.69669829156632090, 56.85652257517428865, 94.99999999999994316 ) ) ;
#2210 = AXIS2_PLACEMENT_3D ( 'NONE', #16391, #16495, #1677 ) ;
#2211 = VECTOR ( 'NONE', #13090, 1000.000000000000114 ) ;
#2212 = CARTESIAN_POINT ( 'NONE',  ( -19.19641293061498999, 381.9323905683720568, -14.20200298773971603 ) ) ;
#2213 = CARTESIAN_POINT ( 'NONE',  ( 88.28695088269886071, 152.5259582928263740, 40.00000000000000000 ) ) ;
#2214 = EDGE_CURVE ( 'NONE', #17585, #2675, #8464, .T. ) ;
#2215 = CARTESIAN_POINT ( 'NONE',  ( -14.54375231895778597, 520.9948905601784190, 14.14213562373094568 ) ) ;
#2216 = CARTESIAN_POINT ( 'NONE',  ( -13.20868407381885845, 339.4948905683720568, -6.410867750099233042 ) ) ;
#2217 = EDGE_CURVE ( 'NONE', #2808, #12831, #9618, .T. ) ;
#2218 = ORIENTED_EDGE ( 'NONE', *, *, #16102, .F. ) ;
#2219 = CARTESIAN_POINT ( 'NONE',  ( -11.93348319268874214, 528.8698905683719431, -2.051577885510841163E-15 ) ) ;
#2220 = ORIENTED_EDGE ( 'NONE', *, *, #18687, .F. ) ;
#2221 = CARTESIAN_POINT ( 'NONE',  ( -11.73070664223724968, 353.1823905601784759, -11.32908994701042715 ) ) ;
#2222 = LINE ( 'NONE', #5664, #12075 ) ;
#2223 = CARTESIAN_POINT ( 'NONE',  ( -48.68588794268870146, 317.2448905601784759, 0.000000000000000000 ) ) ;
#2224 = CARTESIAN_POINT ( 'NONE',  ( -28.68588794268870856, 289.4948905765656377, -19.99999999999999289 ) ) ;
#2225 = CARTESIAN_POINT ( 'NONE',  ( -28.68588794268873343, 494.7448905601785327, -19.99999999999999289 ) ) ;
#2226 = CARTESIAN_POINT ( 'NONE',  ( -25.35362745456400546, 481.0573905683720568, -16.75240474999999307 ) ) ;
#2227 = EDGE_LOOP ( 'NONE', ( #20176, #21132, #15797, #15370 ) ) ;
#2228 = CARTESIAN_POINT ( 'NONE',  ( -13.20868407381887444, 479.4948905683720000, -6.410867750099233042 ) ) ;
#2229 = CARTESIAN_POINT ( 'NONE',  ( -28.68588794268869790, 244.4948905765655809, 19.99999999999999289 ) ) ;
#2230 = AXIS2_PLACEMENT_3D ( 'NONE', #3177, #7912, #9650 ) ;
#2231 = ADVANCED_FACE ( 'NONE', ( #4548 ), #17943, .T. ) ;
#2232 = CARTESIAN_POINT ( 'NONE',  ( -17.35679799567829917, 415.4323905765656377, 16.95518130045146421 ) ) ;
#2233 = CARTESIAN_POINT ( 'NONE',  ( -36.33955658999052929, 473.8698905765656377, 18.47759065022572500 ) ) ;
#2234 = CARTESIAN_POINT ( 'NONE',  ( -28.68588794268872633, 250.8848358243226357, 0.000000000000000000 ) ) ;
#2235 = PLANE ( 'NONE',  #7704 ) ;
#2236 = CARTESIAN_POINT ( 'NONE',  ( 0.5805565836007597902, 3.752776749732560368, -6.499999999999999112 ) ) ;
#2237 = EDGE_CURVE ( 'NONE', #12962, #6677, #21092, .T. ) ;
#2238 = EDGE_CURVE ( 'NONE', #19703, #5058, #16736, .T. ) ;
#2239 = CARTESIAN_POINT ( 'NONE',  ( -48.68588794268871567, 431.9948905765656377, 0.000000000000000000 ) ) ;
#2240 = CARTESIAN_POINT ( 'NONE',  ( 0.4037800551813722216, -4.058962678540097180, 5.969670414742689779 ) ) ;
#2241 = CARTESIAN_POINT ( 'NONE',  ( -28.68588794268870501, 272.8698905683720000, -16.75240474999999307 ) ) ;
#2242 = CARTESIAN_POINT ( 'NONE',  ( -21.03221929538689849, 250.3698905601785043, 18.47759065022572500 ) ) ;
#2243 = CARTESIAN_POINT ( 'NONE',  ( -40.01497788969913216, 363.5573905765655809, 16.95518130045146776 ) ) ;
#2244 = CARTESIAN_POINT ( 'NONE',  ( -16.84014894278199748, 439.1198905683720568, 11.84573899990672530 ) ) ;
#2245 = CARTESIAN_POINT ( 'NONE',  ( -48.68588794268873698, 573.2448905601785327, 0.000000000000000000 ) ) ;
#2246 = CARTESIAN_POINT ( 'NONE',  ( -32.01814843081343298, 267.5573905683720000, 16.75240474999999307 ) ) ;
#2247 = ADVANCED_FACE ( 'NONE', ( #1520 ), #3035, .T. ) ;
#2248 = ORIENTED_EDGE ( 'NONE', *, *, #13331, .F. ) ;
#2249 = CARTESIAN_POINT ( 'NONE',  ( -42.82802356641968089, 535.9948905601785327, -14.14213562373094746 ) ) ;
#2250 = CARTESIAN_POINT ( 'NONE',  ( -40.53162694259545162, 476.6198905683720000, 11.84573899990672885 ) ) ;
#2251 = ORIENTED_EDGE ( 'NONE', *, *, #5318, .F. ) ;
#2252 = CARTESIAN_POINT ( 'NONE',  ( -28.68588794268874054, 573.2448905601785327, 0.000000000000000000 ) ) ;
#2253 = CARTESIAN_POINT ( 'NONE',  ( -19.19641293061497223, 267.3073905683720568, 14.20200298773971426 ) ) ;
#2254 = EDGE_LOOP ( 'NONE', ( #9996, #8480, #4752, #16169 ) ) ;
#2255 = DIRECTION ( 'NONE',  ( 0.000000000000000000, -0.5000000000000018874, -0.8660254037844375974 ) ) ;
#2256 = CARTESIAN_POINT ( 'NONE',  ( -21.03221929538692336, 475.1198905765656377, 18.47759065022572500 ) ) ;
#2257 = CARTESIAN_POINT ( 'NONE',  ( -45.64106924314017988, 388.1823905601784759, 11.32908994701042538 ) ) ;
#2258 = B_SPLINE_CURVE_WITH_KNOTS ( 'NONE', 3,
 ( #5767, #10523, #7786, #9013, #8906, #709, #605, #12374, #18853, #12778, #18639, #19371, #822, #17642, #13904, #11143 ),
 .UNSPECIFIED., .F., .F.,
 ( 4, 2, 2, 2, 2, 2, 2, 4 ),
 ( 0.000000000000000000, 0.001981573912372597106, 0.003963147824745194212, 0.007926295649490388423, 0.009907869561862979457, 0.01188944347423557223, 0.01387101738660816673, 0.01585259129898075950 ),
 .UNSPECIFIED. ) ;
#2259 = CARTESIAN_POINT ( 'NONE',  ( -11.93348319268870661, 240.3698905683720568, -2.051577885510841163E-15 ) ) ;
#2260 =( BOUNDED_CURVE ( )  B_SPLINE_CURVE ( 2, ( #11395, #8040, #14672, #18106, #6524, #21251, #282, #18212, #8253, #14882, #14989, #16608, #19731, #4913, #9771, #16397, #11619 ),
 .UNSPECIFIED., .F., .T. ) 
 B_SPLINE_CURVE_WITH_KNOTS ( ( 3, 2, 2, 2, 2, 2, 2, 2, 3 ),
 ( 0.04687500000000040246, 0.04882812500000036082, 0.05078125000000031919, 0.05273437500000027062, 0.05468750000000022898, 0.05664062500000018735, 0.05859375000000013878, 0.06054687500000009714, 0.06250000000000005551 ),
 .UNSPECIFIED. ) 
 CURVE ( )  GEOMETRIC_REPRESENTATION_ITEM ( )  RATIONAL_B_SPLINE_CURVE ( ( 0.9999999999999960032, 0.9807852804032344274, 1.000000000000000000, 0.9807852804032304306, 1.000000000000000000, 0.9807852804032304306, 1.000000000000000000, 0.9807852804032304306, 1.000000000000000000, 0.9807852804032304306, 1.000000000000000000, 0.9807852804032304306, 1.000000000000000000, 0.9807852804032304306, 1.000000000000000000, 0.9807852804032298755, 1.000000000000000444 ) ) 
 REPRESENTATION_ITEM ( '' )  );
#2261 = CARTESIAN_POINT ( 'NONE',  ( -28.68588794268871567, 374.4948905765656377, 19.99999999999999289 ) ) ;
#2262 = CARTESIAN_POINT ( 'NONE',  ( -42.88789093042841927, 242.9323905683720284, -9.489475012073736337 ) ) ;
#2263 = CARTESIAN_POINT ( 'NONE',  ( -40.53162694259543741, 356.6198905683720000, 11.84573899990672885 ) ) ;
#2264 = CARTESIAN_POINT ( 'NONE',  ( 27.98965548446208373, 333.8848358243226357, 40.00000000000000000 ) ) ;
#2265 =( REPRESENTATION_RELATIONSHIP ('NONE','NONE', #1888, #18847 ) REPRESENTATION_RELATIONSHIP_WITH_TRANSFORMATION ( #8996 )SHAPE_REPRESENTATION_RELATIONSHIP( ) );
#2266 = CARTESIAN_POINT ( 'NONE',  ( -45.43829269268871229, 394.1823905683720000, 3.332260488124734632 ) ) ;
#2267 = CARTESIAN_POINT ( 'NONE',  ( 0.5805565836007647862, 7.505553499465139389, 2.227827669841787811E-16 ) ) ;
#2268 = CARTESIAN_POINT ( 'NONE',  ( -40.01497788969914637, 405.6823905601784759, -16.95518130045146421 ) ) ;
#2269 = ORIENTED_EDGE ( 'NONE', *, *, #15543, .T. ) ;
#2270 = CARTESIAN_POINT ( 'NONE',  ( -28.68588794268874054, 573.2448905601785327, 0.000000000000000000 ) ) ;
#2271 = EDGE_LOOP ( 'NONE', ( #21027, #16797 ) ) ;
#2272 = VERTEX_POINT ( 'NONE', #4859 ) ;
#2273 = CARTESIAN_POINT ( 'NONE',  ( -44.16309181155857999, 505.9948905683720000, 6.410867750099241924 ) ) ;
#2274 = CARTESIAN_POINT ( 'NONE',  ( -8.685887942688713892, 292.2448905601784759, -2.449293598294705724E-15 ) ) ;
#2275 = DIRECTION ( 'NONE',  ( 0.000000000000000000, 0.000000000000000000, -1.000000000000000000 ) ) ;
#2276 = ORIENTED_EDGE ( 'NONE', *, *, #6973, .T. ) ;
#2277 = CARTESIAN_POINT ( 'NONE',  ( -42.88789093042842637, 326.3073905683720568, 9.489475012073734561 ) ) ;
#2278 = CARTESIAN_POINT ( 'NONE',  ( -44.16309181155857289, 353.2448905683720000, -6.410867750099231266 ) ) ;
#2279 = CARTESIAN_POINT ( 'NONE',  ( -44.16309181155856578, 374.4948905683720000, 6.410867750099241924 ) ) ;
#2280 = EDGE_CURVE ( 'NONE', #17485, #9372, #9411, .T. ) ;
#2281 = CARTESIAN_POINT ( 'NONE',  ( -47.16347859291443712, 282.6198905765656377, 7.653668647301805628 ) ) ;
#2282 = DIRECTION ( 'NONE',  ( 0.3090169943749471182, -0.000000000000000000, -0.9510565162951537532 ) ) ;
#2283 = CARTESIAN_POINT ( 'NONE',  ( -32.01814843081343298, 251.6823905683720568, -16.75240474999999307 ) ) ;
#2284 = CARTESIAN_POINT ( 'NONE',  ( 35.96497763894179656, 163.7662197624121632, -60.00000000000000000 ) ) ;
#2285 = CARTESIAN_POINT ( 'NONE',  ( -40.53162694259544452, 424.1198905683720000, -11.84573899990672707 ) ) ;
#2286 = CARTESIAN_POINT ( 'NONE',  ( -48.68588794268870856, 337.2448905601784759, 0.000000000000000000 ) ) ;
#2287 = CARTESIAN_POINT ( 'NONE',  ( -14.54375231895778064, 448.2448905765656377, -14.14213562373094746 ) ) ;
#2288 = PRODUCT_DEFINITION_CONTEXT ( 'detailed design', #7359, 'design' ) ;
#2289 = CARTESIAN_POINT ( 'NONE',  ( 20.42502041961813575, 271.1055109169419666, 40.00000000000000000 ) ) ;
#2290 = CARTESIAN_POINT ( 'NONE',  ( -45.43829269268870519, 325.3698905683720000, 0.000000000000000000 ) ) ;
#2291 = CARTESIAN_POINT ( 'NONE',  ( -25.35362745456399480, 466.6823905683720000, 16.75240474999998952 ) ) ;
#2292 = ORIENTED_EDGE ( 'NONE', *, *, #8145, .F. ) ;
#2293 = CARTESIAN_POINT ( 'NONE',  ( -48.68588794268872277, 467.2448905601784759, 0.000000000000000000 ) ) ;
#2294 = CARTESIAN_POINT ( 'NONE',  ( -14.48388495494898898, 287.9323905683720000, 9.489475012073732785 ) ) ;
#2295 = EDGE_CURVE ( 'NONE', #21097, #1920, #20562, .T. ) ;
#2296 = VERTEX_POINT ( 'NONE', #19787 ) ;
#2297 = CARTESIAN_POINT ( 'NONE',  ( -42.88789093042844058, 444.4323905683720000, -9.489475012073734561 ) ) ;
#2298 = VERTEX_POINT ( 'NONE', #16128 ) ;
#2299 = DIRECTION ( 'NONE',  ( -1.191790137725560488E-16, 1.000000000000000000, -0.000000000000000000 ) ) ;
#2300 = CARTESIAN_POINT ( 'NONE',  ( -28.68588794268870856, 291.3698905683720568, -16.75240474999999307 ) ) ;
#2301 = CARTESIAN_POINT ( 'NONE',  ( -45.43829269268871229, 385.6823905683720000, 3.332260488124734632 ) ) ;
#2302 = VECTOR ( 'NONE', #11935, 1000.000000000000000 ) ;
#2303 = LINE ( 'NONE', #3805, #2804 ) ;
#2304 = CARTESIAN_POINT ( 'NONE',  ( -21.03221929538694468, 518.8698905765655809, -18.47759065022572855 ) ) ;
#2305 = CARTESIAN_POINT ( 'NONE',  ( -42.88789093042844058, 402.9323905683720000, -9.489475012073736337 ) ) ;
#2306 = CARTESIAN_POINT ( 'NONE',  ( -44.16309181155855157, 245.9948905683720284, 6.410867750099241924 ) ) ;
#2307 = CARTESIAN_POINT ( 'NONE',  ( -44.16309181155857289, 434.4948905683720568, 6.410867750099241924 ) ) ;
#2308 = ADVANCED_FACE ( 'NONE', ( #6265 ), #12881, .F. ) ;
#2309 = CIRCLE ( 'NONE', #10225, 175.0000000000000284 ) ;
#2310 = CARTESIAN_POINT ( 'NONE',  ( -17.35679799567829562, 338.5573905765655809, -16.95518130045146421 ) ) ;
#2311 = DIRECTION ( 'NONE',  ( -1.000000000000000000, -0.000000000000000000, -0.000000000000000000 ) ) ;
#2312 = CARTESIAN_POINT ( 'NONE',  ( -19.19641293061497578, 317.3073905683720000, 14.20200298773971426 ) ) ;
#2313 = SHAPE_REPRESENTATION_RELATIONSHIP ( 'NONE' , 'NONE' ,  #3392, #17723 ) ;
#2314 = CARTESIAN_POINT ( 'NONE',  ( -16.84014894278200458, 471.6198905683720000, -11.84573899990672707 ) ) ;
#2315 = DIRECTION ( 'NONE',  ( -0.8090169943749474513, 0.000000000000000000, -0.5877852522924730261 ) ) ;
#2316 = FACE_OUTER_BOUND ( 'NONE', #17897, .T. ) ;
#2317 = LINE ( 'NONE', #7269, #243 ) ;
#2318 = VECTOR ( 'NONE', #15414, 1000.000000000000000 ) ;
#2319 = CARTESIAN_POINT ( 'NONE',  ( -32.01814843081345430, 393.1823905683721136, -16.75240474999999307 ) ) ;
#2320 = CARTESIAN_POINT ( 'NONE',  ( -25.27370346574498683, 45.69746946563440559, -122.4188501256071220 ) ) ;
#2321 = CARTESIAN_POINT ( 'NONE',  ( -21.03221929538694468, 524.1198905601785327, -18.47759065022572855 ) ) ;
#2322 = CARTESIAN_POINT ( 'NONE',  ( -38.17536295476245556, 342.3073905683721136, -14.20200298773971426 ) ) ;
#2323 = VECTOR ( 'NONE', #11187, 1000.000000000000000 ) ;
#2324 = ORIENTED_EDGE ( 'NONE', *, *, #17545, .T. ) ;
#2325 = CARTESIAN_POINT ( 'NONE',  ( -45.43829269268872650, 514.1823905683719431, 3.332260488124734632 ) ) ;
#2326 = EDGE_LOOP ( 'NONE', ( #21282, #8318, #9603, #19499 ) ) ;
#2327 = CARTESIAN_POINT ( 'NONE',  ( -32.66413529028186247, 314.1823905765655809, 19.99999999999999289 ) ) ;
#2328 = DIRECTION ( 'NONE',  ( 1.000000000000000000, 0.000000000000000000, 0.000000000000000000 ) ) ;
#2329 = CYLINDRICAL_SURFACE ( 'NONE', #16267, 19.99999999999999645 ) ;
#2330 = CARTESIAN_POINT ( 'NONE',  ( -42.88789093042844769, 462.9323905683720568, -9.489475012073736337 ) ) ;
#2331 = ORIENTED_EDGE ( 'NONE', *, *, #7194, .F. ) ;
#2332 = CARTESIAN_POINT ( 'NONE',  ( -32.01814843081345430, 496.0573905683720000, 16.75240474999999307 ) ) ;
#2333 = CARTESIAN_POINT ( 'NONE',  ( -32.66413529028185536, 244.1823905765656093, 19.99999999999999289 ) ) ;
#2334 = CIRCLE ( 'NONE', #15463, 20.00000000000000711 ) ;
#2335 = CARTESIAN_POINT ( 'NONE',  ( -11.73070664223725146, 406.0573905765655240, 11.32908994701042005 ) ) ;
#2336 = FACE_BOUND ( 'NONE', #2016, .T. ) ;
#2337 = DIRECTION ( 'NONE',  ( -0.000000000000000000, -1.000000000000000000, -0.000000000000000000 ) ) ;
#2338 = CARTESIAN_POINT ( 'NONE',  ( -48.68588794268872988, 531.9948905765656946, 0.000000000000000000 ) ) ;
#2339 = CARTESIAN_POINT ( 'NONE',  ( -45.64106924314019409, 482.9323905765656377, 11.32908994701042538 ) ) ;
#2340 = AXIS2_PLACEMENT_3D ( 'NONE', #7984, #14613, #21197 ) ;
#2341 =( NAMED_UNIT ( * ) PLANE_ANGLE_UNIT ( ) SI_UNIT ( $, .RADIAN. ) );
#2342 = DIRECTION ( 'NONE',  ( 1.000000000000000000, 0.000000000000000000, 8.901024030850960568E-17 ) ) ;
#2343 = CARTESIAN_POINT ( 'NONE',  ( -19.19641293061497578, 271.9323905683720568, -14.20200298773971603 ) ) ;
#2344 = CARTESIAN_POINT ( 'NONE',  ( -47.16347859291443001, 257.8698905601785327, 7.653668647301805628 ) ) ;
#2345 = DIRECTION ( 'NONE',  ( -0.000000000000000000, -0.000000000000000000, 1.000000000000000000 ) ) ;
#2346 = CARTESIAN_POINT ( 'NONE',  ( -35.09675569278795848, 453.4948905683720568, -15.47720386886985544 ) ) ;
#2347 = CARTESIAN_POINT ( 'NONE',  ( -40.01497788969913927, 330.4323905765655809, -16.95518130045146421 ) ) ;
#2348 = CARTESIAN_POINT ( 'NONE',  ( -28.68588794268870501, 272.8698905683720000, -16.75240474999999307 ) ) ;
#2349 = ADVANCED_FACE ( 'NONE', ( #12979 ), #20992, .T. ) ;
#2350 = ORIENTED_EDGE ( 'NONE', *, *, #6167, .F. ) ;
#2351 = EDGE_LOOP ( 'NONE', ( #17827, #14649, #19605, #7935 ) ) ;
#2352 = CARTESIAN_POINT ( 'NONE',  ( -35.09675569278795848, 493.4948905683720568, -15.47720386886985544 ) ) ;
#2353 = EDGE_CURVE ( 'NONE', #17195, #739, #12770, .T. ) ;
#2354 = ADVANCED_FACE ( 'NONE', ( #14722 ), #6474, .T. ) ;
#2355 = ORIENTED_EDGE ( 'NONE', *, *, #18512, .F. ) ;
#2356 = CARTESIAN_POINT ( 'NONE',  ( -47.16347859291444422, 366.6198905601784759, -7.653668647301793193 ) ) ;
#2357 = CARTESIAN_POINT ( 'NONE',  ( -38.17536295476243424, 235.4323905683720284, 14.20200298773971781 ) ) ;
#2358 = ORIENTED_EDGE ( 'NONE', *, *, #13730, .F. ) ;
#2359 = CARTESIAN_POINT ( 'NONE',  ( -43.68588794268873698, 573.2448905601785327, 0.000000000000000000 ) ) ;
#2360 = CARTESIAN_POINT ( 'NONE',  ( -21.03221929538693757, 478.8698905765656377, -18.47759065022572855 ) ) ;
#2361 = CARTESIAN_POINT ( 'NONE',  ( -36.33955658999051508, 389.1198905601784759, 18.47759065022572500 ) ) ;
#2362 = CARTESIAN_POINT ( 'NONE',  ( 64.58676821086662301, 170.1716627696692683, 57.64290030256307062 ) ) ;
#2363 = CARTESIAN_POINT ( 'NONE',  ( -11.93348319268870661, 230.0573905683720568, 3.332260488124728859 ) ) ;
#2364 = EDGE_CURVE ( 'NONE', #10498, #15904, #14667, .T. ) ;
#2365 = CARTESIAN_POINT ( 'NONE',  ( -42.88789093042845479, 526.3073905683720568, 9.489475012073736337 ) ) ;
#2366 = FACE_OUTER_BOUND ( 'NONE', #20349, .T. ) ;
#2367 = CARTESIAN_POINT ( 'NONE',  ( -44.16309181155855867, 253.2448905683720284, -6.410867750099231266 ) ) ;
#2368 = CARTESIAN_POINT ( 'NONE',  ( -38.17536295476244845, 346.9323905683720568, 14.20200298773971781 ) ) ;
#2369 = CARTESIAN_POINT ( 'NONE',  ( -36.33955658999052929, 469.1198905601784759, 18.47759065022572500 ) ) ;
#2370 = CARTESIAN_POINT ( 'NONE',  ( -14.48388495494900496, 397.9323905683719431, 9.489475012073732785 ) ) ;
#2371 = CARTESIAN_POINT ( 'NONE',  ( -22.30770786884145451, -343.0245277843623057, -122.9933582338429687 ) ) ;
#2372 = CARTESIAN_POINT ( 'NONE',  ( -32.66413529028187668, 379.4323905601785327, 19.99999999999999289 ) ) ;
#2373 = AXIS2_PLACEMENT_3D ( 'NONE', #9376, #17703, #10775 ) ;
#2374 = ORIENTED_EDGE ( 'NONE', *, *, #11940, .T. ) ;
#2375 = DIRECTION ( 'NONE',  ( 0.000000000000000000, 0.000000000000000000, 1.000000000000000000 ) ) ;
#2376 = EDGE_LOOP ( 'NONE', ( #3723, #13311 ) ) ;
#2377 = ORIENTED_EDGE ( 'NONE', *, *, #15674, .F. ) ;
#2378 = CARTESIAN_POINT ( 'NONE',  ( -11.93348319268873858, 500.3698905683720000, -2.051577885510841163E-15 ) ) ;
#2379 = CARTESIAN_POINT ( 'NONE',  ( -48.68588794268870146, 297.2448905601784759, 0.000000000000000000 ) ) ;
#2380 = EDGE_LOOP ( 'NONE', ( #1962, #16194, #18482, #2961 ) ) ;
#2381 = CARTESIAN_POINT ( 'NONE',  ( -32.01814843081344009, 303.1823905683720568, -16.75240474999999307 ) ) ;
#2382 = ORIENTED_EDGE ( 'NONE', *, *, #13800, .F. ) ;
#2383 = CARTESIAN_POINT ( 'NONE',  ( -16.84014894278199037, 350.1198905683720568, -11.84573899990672707 ) ) ;
#2384 = CARTESIAN_POINT ( 'NONE',  ( -32.01814843081344719, 346.0573905683721136, 16.75240474999999307 ) ) ;
#2385 = CARTESIAN_POINT ( 'NONE',  ( -45.64106924314017988, 281.0573905765656377, -11.32908994701042715 ) ) ;
#2386 = DIRECTION ( 'NONE',  ( -0.000000000000000000, 0.000000000000000000, -1.000000000000000000 ) ) ;
#2387 = CARTESIAN_POINT ( 'NONE',  ( -45.43829269268869808, 253.5573905683720000, -3.332260488124726638 ) ) ;
#2388 = CARTESIAN_POINT ( 'NONE',  ( -24.70764059509556176, 464.8073905765656377, 19.99999999999998934 ) ) ;
#2389 = APPLICATION_CONTEXT ( 'automotive_design' ) ;
#2390 = CARTESIAN_POINT ( 'NONE',  ( -14.48388495494900496, 391.3073905683720000, -9.489475012073736337 ) ) ;
#2391 = VECTOR ( 'NONE', #6626, 1000.000000000000000 ) ;
#2392 = DIRECTION ( 'NONE',  ( 0.000000000000000000, 0.000000000000000000, -1.000000000000000000 ) ) ;
#2393 = CARTESIAN_POINT ( 'NONE',  ( -42.82802356641965957, 355.9948905601784759, -14.14213562373094746 ) ) ;
#2394 = DIRECTION ( 'NONE',  ( -1.000000000000000000, 0.000000000000000000, 0.000000000000000000 ) ) ;
#2395 = CARTESIAN_POINT ( 'NONE',  ( -19.19641293061497578, 308.8073905683721136, 14.20200298773971426 ) ) ;
#2396 = CARTESIAN_POINT ( 'NONE',  ( -14.48388495494901385, 469.8073905683719431, -9.489475012073736337 ) ) ;
#2397 = ORIENTED_EDGE ( 'NONE', *, *, #21201, .T. ) ;
#2398 = CARTESIAN_POINT ( 'NONE',  ( -24.70764059509557597, 474.4323905601785327, -19.99999999999999289 ) ) ;
#2399 = CARTESIAN_POINT ( 'NONE',  ( -11.93348319268871371, 288.5573905683720000, 3.332260488124728415 ) ) ;
#2400 = EDGE_CURVE ( 'NONE', #13902, #14194, #12740, .T. ) ;
#2401 = ORIENTED_EDGE ( 'NONE', *, *, #4850, .T. ) ;
#2402 = CARTESIAN_POINT ( 'NONE',  ( -8.685887942688724550, 376.9948905765655809, -2.449293598294705724E-15 ) ) ;
#2403 = VERTEX_POINT ( 'NONE', #16555 ) ;
#2404 = ORIENTED_EDGE ( 'NONE', *, *, #21120, .T. ) ;
#2405 = CARTESIAN_POINT ( 'NONE',  ( 20.42502041961813930, 230.5765313837437418, -49.99999999999999289 ) ) ;
#2406 = CARTESIAN_POINT ( 'NONE',  ( -10.20829729246298356, 342.8698905601785327, -7.653668647301794969 ) ) ;
#2407 = CARTESIAN_POINT ( 'NONE',  ( -28.68588794268870856, 301.3698905683720568, -16.75240474999999307 ) ) ;
#2408 = AXIS2_PLACEMENT_3D ( 'NONE', #3130, #1404, #3240 ) ;
#2409 = CARTESIAN_POINT ( 'NONE',  ( -45.43829269268871229, 385.0573905683720000, -3.332260488124726638 ) ) ;
#2410 = DIRECTION ( 'NONE',  ( 0.3090169943749471182, -0.000000000000000000, -0.9510565162951537532 ) ) ;
#2411 = EDGE_CURVE ( 'NONE', #629, #2934, #19362, .T. ) ;
#2412 = CARTESIAN_POINT ( 'NONE',  ( -24.70764059509556887, 514.8073905765656946, 19.99999999999998934 ) ) ;
#2413 = CARTESIAN_POINT ( 'NONE',  ( -13.20868407381886556, 409.4948905683720000, -6.410867750099233042 ) ) ;
#2414 = CARTESIAN_POINT ( 'NONE',  ( -19.19641293061496867, 238.8073905683720000, 14.20200298773971426 ) ) ;
#2415 = CARTESIAN_POINT ( 'NONE',  ( -42.88789093042844058, 414.8073905683720000, 9.489475012073734561 ) ) ;
#2416 = CARTESIAN_POINT ( 'NONE',  ( -28.68588794268871212, 339.4948905765656377, -19.99999999999999289 ) ) ;
#2417 = CARTESIAN_POINT ( 'NONE',  ( 69.55855958429435759, 152.5125485459294623, 64.92624364808513349 ) ) ;
#2418 = CARTESIAN_POINT ( 'NONE',  ( -16.84014894278198327, 300.1198905683720000, -11.84573899990672707 ) ) ;
#2419 = DIRECTION ( 'NONE',  ( 0.000000000000000000, 0.000000000000000000, 1.000000000000000000 ) ) ;
#2420 = CARTESIAN_POINT ( 'NONE',  ( -11.93348319268873503, 470.3698905683720568, -2.051577885510841163E-15 ) ) ;
#2421 = CARTESIAN_POINT ( 'NONE',  ( -11.73070664223726567, 516.0573905765655809, 11.32908994701042005 ) ) ;
#2422 = DIRECTION ( 'NONE',  ( 0.4627175328665443232, 5.514621922230504147E-17, 0.8865057725575725689 ) ) ;
#2423 = DIRECTION ( 'NONE',  ( -1.000000000000000000, 0.000000000000000000, 0.000000000000000000 ) ) ;
#2424 = CARTESIAN_POINT ( 'NONE',  ( -19.19641293061498288, 368.8073905683720000, 14.20200298773971426 ) ) ;
#2425 = DIRECTION ( 'NONE',  ( 1.191790137725560488E-16, -1.000000000000000000, -0.000000000000000000 ) ) ;
#2426 = CARTESIAN_POINT ( 'NONE',  ( -28.68588794268873343, 529.7448905601785327, 19.99999999999999289 ) ) ;
#2427 = CARTESIAN_POINT ( 'NONE',  ( -45.43829269268870519, 343.5573905683720000, -3.332260488124726194 ) ) ;
#2428 = ADVANCED_FACE ( 'NONE', ( #13415 ), #1739, .F. ) ;
#2429 = ORIENTED_EDGE ( 'NONE', *, *, #331, .F. ) ;
#2430 = CARTESIAN_POINT ( 'NONE',  ( -28.68588794268873343, 501.3698905683721136, -16.75240474999999307 ) ) ;
#2431 = EDGE_LOOP ( 'NONE', ( #845, #5187, #3987, #17616, #13939 ) ) ;
#2432 = AXIS2_PLACEMENT_3D ( 'NONE', #9762, #19404, #16171 ) ;
#2433 = CARTESIAN_POINT ( 'NONE',  ( -45.64106924314017988, 381.0573905765656377, -11.32908994701042538 ) ) ;
#2434 = CARTESIAN_POINT ( 'NONE',  ( 5.299999999999999822, 3.752776749732560368, -6.499999999999999112 ) ) ;
#2435 = CARTESIAN_POINT ( 'NONE',  ( -8.685887942688625074, 287.3073905765656377, -3.978247347592952732 ) ) ;
#2436 = DIRECTION ( 'NONE',  ( 1.000000000000000000, 0.000000000000000000, 0.000000000000000000 ) ) ;
#2437 = CARTESIAN_POINT ( 'NONE',  ( -14.48388495494900852, 457.9323905683720568, 9.489475012073732785 ) ) ;
#2438 = ORIENTED_EDGE ( 'NONE', *, *, #3669, .T. ) ;
#2439 = CARTESIAN_POINT ( 'NONE',  ( -25.35362745456399480, 476.6823905683720000, 16.75240474999998952 ) ) ;
#2440 = CARTESIAN_POINT ( 'NONE',  ( 69.79185940953689737, 142.2976266388001250, 69.11456258820065557 ) ) ;
#2441 = CARTESIAN_POINT ( 'NONE',  ( -8.685887942688726326, 406.6823905765656377, 3.978247347593161010 ) ) ;
#2442 = DIRECTION ( 'NONE',  ( 1.000000000000000000, 0.000000000000000000, 0.000000000000000000 ) ) ;
#2443 = CARTESIAN_POINT ( 'NONE',  ( -28.68588794268874054, 573.2448905601785327, 0.000000000000000000 ) ) ;
#2444 = FACE_OUTER_BOUND ( 'NONE', #15870, .T. ) ;
#2445 = CARTESIAN_POINT ( 'NONE',  ( -28.68588794268874054, 573.2448905601785327, 0.000000000000000000 ) ) ;
#2446 = EDGE_CURVE ( 'NONE', #9937, #182, #19895, .T. ) ;
#2447 = CIRCLE ( 'NONE', #14538, 125.0000000000000000 ) ;
#2448 = LINE ( 'NONE', #5678, #9563 ) ;
#2449 = CARTESIAN_POINT ( 'NONE',  ( 10.41669750159067220, 217.7548513357008630, 60.00000000000000000 ) ) ;
#2450 = CLOSED_SHELL ( 'NONE', ( #19758, #11324, #20934, #6664, #18208, #6389 ) ) ;
#2451 = CARTESIAN_POINT ( 'NONE',  ( -45.43829269268869808, 285.6823905683720000, 3.332260488124734632 ) ) ;
#2452 = CARTESIAN_POINT ( 'NONE',  ( -48.68588794268871567, 401.9948905765656377, 0.000000000000000000 ) ) ;
#2453 = CARTESIAN_POINT ( 'NONE',  ( -44.16309181155857289, 445.9948905683720568, 6.410867750099241924 ) ) ;
#2454 = LINE ( 'NONE', #18989, #5756 ) ;
#2455 = CARTESIAN_POINT ( 'NONE',  ( -13.20868407381884779, 279.7448905683720568, 6.410867750099229490 ) ) ;
#2456 = ADVANCED_FACE ( 'NONE', ( #11886 ), #16770, .F. ) ;
#2457 = EDGE_LOOP ( 'NONE', ( #14566, #789, #6059, #11333 ) ) ;
#2458 = CARTESIAN_POINT ( 'NONE',  ( -32.66413529028188378, 479.8073905765656377, -19.99999999999999289 ) ) ;
#2459 = ORIENTED_EDGE ( 'NONE', *, *, #11869, .F. ) ;
#2460 = CARTESIAN_POINT ( 'NONE',  ( -14.48388495494901029, 481.3073905683720000, -9.489475012073734561 ) ) ;
#2461 = AXIS2_PLACEMENT_3D ( 'NONE', #12365, #917, #4252 ) ;
#2462 = ORIENTED_EDGE ( 'NONE', *, *, #7649, .T. ) ;
#2463 = CARTESIAN_POINT ( 'NONE',  ( -11.73070664223724968, 363.1823905601784759, -11.32908994701042538 ) ) ;
#2464 = CARTESIAN_POINT ( 'NONE',  ( -13.20868407381884602, 238.2448905683720000, 6.410867750099229490 ) ) ;
#2465 = ORIENTED_EDGE ( 'NONE', *, *, #1622, .T. ) ;
#2466 = LINE ( 'NONE', #17179, #15585 ) ;
#2467 = CARTESIAN_POINT ( 'NONE',  ( -11.73070664223725856, 466.0573905765656946, 11.32908994701042005 ) ) ;
#2468 = CARTESIAN_POINT ( 'NONE',  ( 69.79185940953689737, 142.2976266388001250, -69.11456258820064136 ) ) ;
#2469 = DIRECTION ( 'NONE',  ( -0.000000000000000000, -1.000000000000000000, -0.000000000000000000 ) ) ;
#2470 = CARTESIAN_POINT ( 'NONE',  ( 1.336753550880579347E-14, 213.9102039777116602, -25.00000000000000000 ) ) ;
#2471 = CARTESIAN_POINT ( 'NONE',  ( -11.93348319268874036, 520.6823905683719431, -3.332260488124732856 ) ) ;
#2472 = CARTESIAN_POINT ( 'NONE',  ( -14.54375231895776821, 375.7448905765656377, 14.14213562373094568 ) ) ;
#2473 = CARTESIAN_POINT ( 'NONE',  ( -16.84014894278197261, 247.6198905683720284, 11.84573899990672530 ) ) ;
#2474 = CARTESIAN_POINT ( 'NONE',  ( -25.35362745456397704, 338.1823905683720000, 16.75240474999998952 ) ) ;
#2475 = CARTESIAN_POINT ( 'NONE',  ( -8.685887942688742314, 573.2448905601785327, 2.449293598294706119E-15 ) ) ;
#2476 = CARTESIAN_POINT ( 'NONE',  ( -24.70764059509554045, 304.8073905765655809, 19.99999999999998934 ) ) ;
#2477 = CARTESIAN_POINT ( 'NONE',  ( -42.88789093042843348, 382.9323905683720568, -9.489475012073736337 ) ) ;
#2478 = CARTESIAN_POINT ( 'NONE',  ( -11.73070664223724258, 326.0573905765656377, 11.32908994701042005 ) ) ;
#2479 = EDGE_CURVE ( 'NONE', #11401, #5772, #10149, .T. ) ;
#2480 = CARTESIAN_POINT ( 'NONE',  ( -45.64106924314018698, 388.1823905601784759, 11.32908994701042715 ) ) ;
#2481 = EDGE_CURVE ( 'NONE', #19827, #7658, #18157, .T. ) ;
#2482 = DIRECTION ( 'NONE',  ( 0.000000000000000000, 1.000000000000000000, 0.000000000000000000 ) ) ;
#2483 = ORIENTED_EDGE ( 'NONE', *, *, #8756, .T. ) ;
#2484 = ORIENTED_EDGE ( 'NONE', *, *, #14921, .T. ) ;
#2485 = CARTESIAN_POINT ( 'NONE',  ( -40.53162694259545873, 506.6198905683721136, 11.84573899990672885 ) ) ;
#2486 = CARTESIAN_POINT ( 'NONE',  ( -40.01497788969912506, 293.5573905765655809, 16.95518130045146776 ) ) ;
#2487 = ORIENTED_EDGE ( 'NONE', *, *, #5141, .F. ) ;
#2488 = CARTESIAN_POINT ( 'NONE',  ( -11.93348319268871371, 300.0573905683720568, 3.332260488124728859 ) ) ;
#2489 = PRODUCT_RELATED_PRODUCT_CATEGORY ( 'part', '', ( #4407 ) ) ;
#2490 = AXIS2_PLACEMENT_3D ( 'NONE', #11203, #6119, #7841 ) ;
#2491 = ORIENTED_EDGE ( 'NONE', *, *, #5373, .T. ) ;
#2492 = CARTESIAN_POINT ( 'NONE',  ( -44.16309181155856578, 344.4948905683720000, 6.410867750099241924 ) ) ;
#2493 = CARTESIAN_POINT ( 'NONE',  ( -19.19641293061497933, 340.4323905683720568, -14.20200298773971603 ) ) ;
#2494 = CARTESIAN_POINT ( 'NONE',  ( -21.03221929538691626, 288.8698905765656377, -18.47759065022572855 ) ) ;
#2495 = LINE ( 'NONE', #2711, #8951 ) ;
#2496 = CARTESIAN_POINT ( 'NONE',  ( -22.27502019258946220, 246.9948905683720284, 15.47720386886985189 ) ) ;
#2497 = CARTESIAN_POINT ( 'NONE',  ( -47.16347859291445843, 462.6198905765655809, 7.653668647301805628 ) ) ;
#2498 = CARTESIAN_POINT ( 'NONE',  ( -38.17536295476245556, 396.9323905683721136, 14.20200298773971781 ) ) ;
#2499 = LINE ( 'NONE', #783, #977 ) ;
#2500 = CARTESIAN_POINT ( 'NONE',  ( -11.73070664223726034, 447.9323905765656946, -11.32908994701042538 ) ) ;
#2501 = DIRECTION ( 'NONE',  ( 1.374938938973709817E-16, -1.000000000000000000, 0.000000000000000000 ) ) ;
#2502 = CARTESIAN_POINT ( 'NONE',  ( -25.35362745456400191, 441.0573905683720000, -16.75240474999999307 ) ) ;
#2503 = ORIENTED_EDGE ( 'NONE', *, *, #9742, .F. ) ;
#2504 = CIRCLE ( 'NONE', #4571, 4.000000000000000000 ) ;
#2505 = CARTESIAN_POINT ( 'NONE',  ( -45.64106924314019409, 448.1823905601785327, 11.32908994701042715 ) ) ;
#2506 = VERTEX_POINT ( 'NONE', #3769 ) ;
#2507 = DIRECTION ( 'NONE',  ( -1.000000000000000000, -0.000000000000000000, -0.000000000000000000 ) ) ;
#2508 = ORIENTED_EDGE ( 'NONE', *, *, #5828, .T. ) ;
#2509 = ORIENTED_EDGE ( 'NONE', *, *, #16551, .T. ) ;
#2510 = DIRECTION ( 'NONE',  ( 1.000000000000000000, 0.000000000000000000, -0.000000000000000000 ) ) ;
#2511 = CARTESIAN_POINT ( 'NONE',  ( -36.33955658999050087, 325.3698905601784759, -18.47759065022572855 ) ) ;
#2512 = CARTESIAN_POINT ( 'NONE',  ( -45.43829269268869808, 304.1823905683720568, 3.332260488124734632 ) ) ;
#2513 = CARTESIAN_POINT ( 'NONE',  ( -44.16309181155856578, 355.9948905683720000, 6.410867750099241924 ) ) ;
#2514 = CARTESIAN_POINT ( 'NONE',  ( -46.31968306282883674, 326.0737056351150613, -33.59072564020502938 ) ) ;
#2515 = CARTESIAN_POINT ( 'NONE',  ( -11.73070664223727100, 527.9323905765655809, -11.32908994701042715 ) ) ;
#2516 = CARTESIAN_POINT ( 'NONE',  ( -19.19641293061498999, 400.4323905683720568, -14.20200298773971603 ) ) ;
#2517 = CARTESIAN_POINT ( 'NONE',  ( -14.48388495494898365, 231.3073905683720000, -9.489475012073736337 ) ) ;
#2518 = VECTOR ( 'NONE', #8598, 1000.000000000000000 ) ;
#2519 = CARTESIAN_POINT ( 'NONE',  ( -38.17536295476245556, 405.4323905683721136, 14.20200298773971781 ) ) ;
#2520 = CONTEXT_DEPENDENT_SHAPE_REPRESENTATION ( #5978, #20987 ) ;
#2521 = CARTESIAN_POINT ( 'NONE',  ( -48.68588794268870856, 341.6823905765656946, -3.978247347593158345 ) ) ;
#2522 = CARTESIAN_POINT ( 'NONE',  ( -28.68588794268871212, 324.7448905601784759, -19.99999999999999289 ) ) ;
#2523 = CARTESIAN_POINT ( 'NONE',  ( -16.84014894278198327, 310.1198905683720000, -11.84573899990672707 ) ) ;
#2524 = CARTESIAN_POINT ( 'NONE',  ( -38.17536295476246977, 463.8073905683720000, -14.20200298773971426 ) ) ;
#2525 = CARTESIAN_POINT ( 'NONE',  ( -40.01497788969915348, 513.5573905765656946, 16.95518130045146776 ) ) ;
#2526 = CYLINDRICAL_SURFACE ( 'NONE', #15944, 4.000000000000000000 ) ;
#2527 = AXIS2_PLACEMENT_3D ( 'NONE', #55, #10190, #377 ) ;
#2528 = DIRECTION ( 'NONE',  ( -1.191790137725560488E-16, 1.000000000000000000, -0.000000000000000000 ) ) ;
#2529 = CARTESIAN_POINT ( 'NONE',  ( -42.88789093042843348, 364.4323905683720568, -9.489475012073736337 ) ) ;
#2530 = PLANE ( 'NONE',  #13028 ) ;
#2531 = CARTESIAN_POINT ( 'NONE',  ( -17.35679799567830983, 500.6823905601785327, 16.95518130045146421 ) ) ;
#2532 = CARTESIAN_POINT ( 'NONE',  ( -35.09675569278794427, 341.9948905683720000, -15.47720386886985544 ) ) ;
#2533 = EDGE_LOOP ( 'NONE', ( #12722, #17671, #818, #18378, #1752, #7518, #987, #19029 ) ) ;
#2534 = CARTESIAN_POINT ( 'NONE',  ( -32.01814843081346851, 511.6823905683720000, -16.75240474999999307 ) ) ;
#2535 = VERTEX_POINT ( 'NONE', #10356 ) ;
#2536 = DIRECTION ( 'NONE',  ( 0.000000000000000000, 0.000000000000000000, -1.000000000000000000 ) ) ;
#2537 = CARTESIAN_POINT ( 'NONE',  ( -45.43829269268871940, 415.0573905683721136, -3.332260488124726638 ) ) ;
#2538 = CARTESIAN_POINT ( 'NONE',  ( 4.700000000000000178, 3.752776749732563033, 6.500000000000000000 ) ) ;
#2539 = DIRECTION ( 'NONE',  ( 0.000000000000000000, 1.000000000000000000, 0.000000000000000000 ) ) ;
#2540 = CARTESIAN_POINT ( 'NONE',  ( -45.43829269268871940, 464.1823905683720568, 3.332260488124734632 ) ) ;
#2541 = ORIENTED_EDGE ( 'NONE', *, *, #12879, .T. ) ;
#2542 = CARTESIAN_POINT ( 'NONE',  ( -13.20868407381887266, 459.4948905683720568, -6.410867750099233042 ) ) ;
#2543 = CARTESIAN_POINT ( 'NONE',  ( -48.68588794268869435, 241.9948905765656377, 0.000000000000000000 ) ) ;
#2544 = VECTOR ( 'NONE', #16108, 1000.000000000000114 ) ;
#2545 = CARTESIAN_POINT ( 'NONE',  ( -17.35679799567829562, 395.4323905765655809, 16.95518130045146421 ) ) ;
#2546 = CYLINDRICAL_SURFACE ( 'NONE', #20699, 4.000000000000001776 ) ;
#2547 = CARTESIAN_POINT ( 'NONE',  ( -48.68588794268870856, 371.9948905765655809, 0.000000000000000000 ) ) ;
#2548 = CARTESIAN_POINT ( 'NONE',  ( 40.42502041961814996, 180.1716627696692967, -40.00000000000000000 ) ) ;
#2549 = LINE ( 'NONE', #10536, #104 ) ;
#2550 = AXIS2_PLACEMENT_3D ( 'NONE', #3376, #13110, #20134 ) ;
#2551 = EDGE_CURVE ( 'NONE', #19677, #7489, #18797, .T. ) ;
#2552 = CARTESIAN_POINT ( 'NONE',  ( -165.7253922195053235, 585.7448905601785327, 108.8355377051282176 ) ) ;
#2553 = CARTESIAN_POINT ( 'NONE',  ( -48.68588794268869435, 237.2448905601785043, 0.000000000000000000 ) ) ;
#2554 = LINE ( 'NONE', #8817, #1775 ) ;
#2555 = CARTESIAN_POINT ( 'NONE',  ( -19.19641293061497223, 278.8073905683720000, 14.20200298773971426 ) ) ;
#2556 = LINE ( 'NONE', #20834, #5748 ) ;
#2557 = CARTESIAN_POINT ( 'NONE',  ( -13.20868407381886911, 430.9948905683720568, -6.410867750099233042 ) ) ;
#2558 = CARTESIAN_POINT ( 'NONE',  ( -10.20829729246299067, 397.6198905765655809, -7.653668647301794969 ) ) ;
#2559 = CARTESIAN_POINT ( 'NONE',  ( -11.93348319268871194, 280.0573905683720568, 3.332260488124728415 ) ) ;
#2560 = VERTEX_POINT ( 'NONE', #979 ) ;
#2561 = CARTESIAN_POINT ( 'NONE',  ( -11.73070664223726389, 477.9323905765656946, -11.32908994701042538 ) ) ;
#2562 = EDGE_LOOP ( 'NONE', ( #9288, #20647, #11571, #14040, #16782, #6294, #19627, #4293, #4499, #12669, #13046, #8315, #11460, #12863, #19706, #8488, #3063, #6641, #7418, #12835, #14389 ) ) ;
#2563 = CARTESIAN_POINT ( 'NONE',  ( -44.16309181155857999, 485.9948905683720568, 6.410867750099241924 ) ) ;
#2564 = AXIS2_PLACEMENT_3D ( 'NONE', #7882, #9824, #19676 ) ;
#2565 = EDGE_CURVE ( 'NONE', #2808, #469, #20868, .T. ) ;
#2566 = ORIENTED_EDGE ( 'NONE', *, *, #12043, .F. ) ;
#2567 = CARTESIAN_POINT ( 'NONE',  ( -17.35679799567829562, 363.8073905601784759, -16.95518130045146421 ) ) ;
#2568 = CARTESIAN_POINT ( 'NONE',  ( -45.43829269268869098, 233.5573905683720568, -3.332260488124726194 ) ) ;
#2569 = ORIENTED_EDGE ( 'NONE', *, *, #10096, .T. ) ;
#2570 =( BOUNDED_CURVE ( )  B_SPLINE_CURVE ( 2, ( #14302, #15914, #11134, #19358, #1105, #15704, #9509, #20561, #786, #6053, #19256, #11022, #891, #17632, #12340, #14407, #20989 ),
 .UNSPECIFIED., .F., .T. ) 
 B_SPLINE_CURVE_WITH_KNOTS ( ( 3, 2, 2, 2, 2, 2, 2, 2, 3 ),
 ( 0.06250000000000005551, 0.06445312500000009714, 0.06640625000000015266, 0.06835937500000019429, 0.07031250000000024980, 0.07226562500000029143, 0.07421875000000033307, 0.07617187500000038858, 0.07812500000000043021 ),
 .UNSPECIFIED. ) 
 CURVE ( )  GEOMETRIC_REPRESENTATION_ITEM ( )  RATIONAL_B_SPLINE_CURVE ( ( 0.9999999999999994449, 0.9807852804032309857, 1.000000000000000000, 0.9807852804032304306, 1.000000000000000000, 0.9807852804032304306, 1.000000000000000000, 0.9807852804032304306, 1.000000000000000000, 0.9807852804032304306, 1.000000000000000000, 0.9807852804032304306, 1.000000000000000000, 0.9807852804032304306, 1.000000000000000000, 0.9807852804032262117, 1.000000000000004219 ) ) 
 REPRESENTATION_ITEM ( '' )  );
#2571 = CARTESIAN_POINT ( 'NONE',  ( -40.53162694259545873, 522.6198905683720568, -11.84573899990672707 ) ) ;
#2572 = DIRECTION ( 'NONE',  ( 1.000000000000000000, 0.000000000000000000, 0.000000000000000000 ) ) ;
#2573 = CARTESIAN_POINT ( 'NONE',  ( -8.685887942688736985, 466.6823905765656946, 3.978247347593161010 ) ) ;
#2574 = FACE_OUTER_BOUND ( 'NONE', #10637, .T. ) ;
#2575 = CARTESIAN_POINT ( 'NONE',  ( -36.33955658999050797, 283.8698905765656377, 18.47759065022572500 ) ) ;
#2576 = CARTESIAN_POINT ( 'NONE',  ( -42.82802356641967378, 455.9948905601784759, -14.14213562373094746 ) ) ;
#2577 = CARTESIAN_POINT ( 'NONE',  ( 20.42502041961813575, 271.1055109169419666, 40.00000000000000000 ) ) ;
#2578 = EDGE_CURVE ( 'NONE', #5772, #12831, #20182, .T. ) ;
#2579 = CARTESIAN_POINT ( 'NONE',  ( -28.68588794268873698, 522.8698905683719431, -16.75240474999999307 ) ) ;
#2580 = LINE ( 'NONE', #754, #4557 ) ;
#2581 = DIRECTION ( 'NONE',  ( 0.000000000000000000, 0.000000000000000000, 1.000000000000000000 ) ) ;
#2582 = CARTESIAN_POINT ( 'NONE',  ( -11.93348319268870839, 248.5573905683719715, 3.332260488124728415 ) ) ;
#2583 = CARTESIAN_POINT ( 'NONE',  ( -44.16309181155856578, 345.9948905683720000, 6.410867750099241924 ) ) ;
#2584 = DIRECTION ( 'NONE',  ( -1.191790137725560488E-16, 1.000000000000000000, -0.000000000000000000 ) ) ;
#2585 = CARTESIAN_POINT ( 'NONE',  ( -40.01497788969912506, 303.5573905765656377, 16.95518130045146776 ) ) ;
#2586 = CARTESIAN_POINT ( 'NONE',  ( -13.20868407381886378, 389.4948905683720000, -6.410867750099233042 ) ) ;
#2587 = DIRECTION ( 'NONE',  ( 0.000000000000000000, 0.000000000000000000, 1.000000000000000000 ) ) ;
#2588 = CARTESIAN_POINT ( 'NONE',  ( -21.03221929538691271, 380.3698905601784759, 18.47759065022572500 ) ) ;
#2589 = VERTEX_POINT ( 'NONE', #12096 ) ;
#2590 = DIRECTION ( 'NONE',  ( 1.000000000000000000, 0.000000000000000000, 0.000000000000000000 ) ) ;
#2591 = ORIENTED_EDGE ( 'NONE', *, *, #21349, .F. ) ;
#2592 = ORIENTED_EDGE ( 'NONE', *, *, #8743, .F. ) ;
#2593 = CARTESIAN_POINT ( 'NONE',  ( -14.48388495494901562, 499.4323905683720000, 9.489475012073732785 ) ) ;
#2594 = CARTESIAN_POINT ( 'NONE',  ( -28.68588794268874054, 573.2448905601785327, 0.000000000000000000 ) ) ;
#2595 = ORIENTED_EDGE ( 'NONE', *, *, #6720, .T. ) ;
#2596 = CARTESIAN_POINT ( 'NONE',  ( -38.17536295476244135, 306.9323905683719431, 14.20200298773971781 ) ) ;
#2597 = ORIENTED_EDGE ( 'NONE', *, *, #20952, .T. ) ;
#2598 = CARTESIAN_POINT ( 'NONE',  ( -22.27502019258948707, 350.7448905683720568, -15.47720386886985544 ) ) ;
#2599 = CARTESIAN_POINT ( 'NONE',  ( -35.09675569278794427, 341.9948905683720000, -15.47720386886985544 ) ) ;
#2600 = CARTESIAN_POINT ( 'NONE',  ( -10.20829729246297646, 286.3698905765655809, 7.653668647301790529 ) ) ;
#2601 = CYLINDRICAL_SURFACE ( 'NONE', #3439, 19.99999999999999645 ) ;
#2602 = CARTESIAN_POINT ( 'NONE',  ( -11.93348319268870661, 238.8698905683720568, -2.051577885510841163E-15 ) ) ;
#2603 = CARTESIAN_POINT ( 'NONE',  ( -21.03221929538690560, 224.1198905601785043, -18.47759065022572855 ) ) ;
#2604 = CARTESIAN_POINT ( 'NONE',  ( -22.27502019258949062, 392.2448905683720568, -15.47720386886985544 ) ) ;
#2605 = FACE_OUTER_BOUND ( 'NONE', #14439, .T. ) ;
#2606 = DIRECTION ( 'NONE',  ( 0.000000000000000000, -0.000000000000000000, -1.000000000000000000 ) ) ;
#2607 = LINE ( 'NONE', #5840, #13238 ) ;
#2608 = CARTESIAN_POINT ( 'NONE',  ( -11.93348319268873148, 449.1823905683720000, -3.332260488124732856 ) ) ;
#2609 = ORIENTED_EDGE ( 'NONE', *, *, #10014, .T. ) ;
#2610 = CARTESIAN_POINT ( 'NONE',  ( -45.64106924314019409, 438.1823905601784190, 11.32908994701042715 ) ) ;
#2611 = EDGE_CURVE ( 'NONE', #18039, #6038, #13957, .T. ) ;
#2612 = ORIENTED_EDGE ( 'NONE', *, *, #5110, .T. ) ;
#2613 = VERTEX_POINT ( 'NONE', #7542 ) ;
#2614 = VERTEX_POINT ( 'NONE', #2267 ) ;
#2615 = DIRECTION ( 'NONE',  ( 1.000000000000000000, 0.000000000000000000, -0.000000000000000000 ) ) ;
#2616 = CARTESIAN_POINT ( 'NONE',  ( -45.64106924314017988, 316.3073905601784759, -11.32908994701042715 ) ) ;
#2617 = EDGE_CURVE ( 'NONE', #2082, #10139, #12035, .T. ) ;
#2618 = ADVANCED_FACE ( 'NONE', ( #20756 ), #9061, .F. ) ;
#2619 = CARTESIAN_POINT ( 'NONE',  ( -35.09675569278794427, 363.4948905683720568, -15.47720386886985544 ) ) ;
#2620 = DIRECTION ( 'NONE',  ( 0.000000000000000000, 0.000000000000000000, 1.000000000000000000 ) ) ;
#2621 = CARTESIAN_POINT ( 'NONE',  ( -48.68588794268872988, 521.6823905765656946, -3.978247347593158345 ) ) ;
#2622 = CARTESIAN_POINT ( 'NONE',  ( -32.01814843081345430, 401.6823905683720000, -16.75240474999999307 ) ) ;
#2623 = CARTESIAN_POINT ( 'NONE',  ( -11.93348319268870661, 250.3698905683720000, -2.051577885510841163E-15 ) ) ;
#2624 = CARTESIAN_POINT ( 'NONE',  ( -25.35362745456398414, 396.6823905683720000, 16.75240474999998952 ) ) ;
#2625 = B_SPLINE_CURVE_WITH_KNOTS ( 'NONE', 3,
 ( #11318, #8168, #1488, #12738, #1596, #1383, #17913, #17603, #17708, #14800, #21384, #7853, #9380, #15998, #20960, #6131, #19330, #9486 ),
 .UNSPECIFIED., .F., .F.,
 ( 4, 2, 2, 2, 2, 2, 2, 2, 4 ),
 ( 0.1916473082429159536, 0.2301913947125514559, 0.2687354811821869305, 0.3072795676518224606, 0.3458236541214579907, 0.3843677405910934652, 0.4229118270607289398, 0.4614559135303645254, 0.5000000000000000000 ),
 .UNSPECIFIED. ) ;
#2626 = CARTESIAN_POINT ( 'NONE',  ( -8.685887942688720997, 336.9948905765656377, -2.449293598294705724E-15 ) ) ;
#2627 = CARTESIAN_POINT ( 'NONE',  ( -36.33955658999050087, 325.3698905601784759, -18.47759065022572855 ) ) ;
#2628 = CARTESIAN_POINT ( 'NONE',  ( -32.01814843081344009, 316.0573905683720000, 16.75240474999999307 ) ) ;
#2629 = SHAPE_REPRESENTATION_RELATIONSHIP ( 'NONE' , 'NONE' ,  #10694, #21324 ) ;
#2630 = CARTESIAN_POINT ( 'NONE',  ( -32.01814843081346140, 453.1823905683720568, -16.75240474999999307 ) ) ;
#2631 = EDGE_CURVE ( 'NONE', #17585, #2829, #14280, .T. ) ;
#2632 = CARTESIAN_POINT ( 'NONE',  ( -48.68588794268872988, 511.9948905765656377, 0.000000000000000000 ) ) ;
#2633 = LINE ( 'NONE', #17762, #7965 ) ;
#2634 = DIRECTION ( 'NONE',  ( 0.000000000000000000, 0.000000000000000000, -1.000000000000000000 ) ) ;
#2635 = CARTESIAN_POINT ( 'NONE',  ( -22.27502019258950128, 500.7448905683720000, -15.47720386886985544 ) ) ;
#2636 = CARTESIAN_POINT ( 'NONE',  ( -17.35679799567830983, 510.6823905601785327, 16.95518130045146421 ) ) ;
#2637 = CARTESIAN_POINT ( 'NONE',  ( -42.88789093042842637, 324.8073905683720000, 9.489475012073736337 ) ) ;
#2638 = ORIENTED_EDGE ( 'NONE', *, *, #3136, .T. ) ;
#2639 = CARTESIAN_POINT ( 'NONE',  ( -45.43829269268872650, 513.5573905683719431, -3.332260488124726194 ) ) ;
#2640 = VERTEX_POINT ( 'NONE', #15790 ) ;
#2641 = B_SPLINE_CURVE_WITH_KNOTS ( 'NONE', 3,
 ( #21002, #9201, #19269, #19168, #1011, #106 ),
 .UNSPECIFIED., .F., .F.,
 ( 4, 2, 4 ),
 ( 2.380733003134506766E-07, 0.001898835937927388726, 0.003797433802554464090 ),
 .UNSPECIFIED. ) ;
#2642 = FACE_BOUND ( 'NONE', #18140, .T. ) ;
#2643 = VECTOR ( 'NONE', #2908, 1000.000000000000000 ) ;
#2644 = CARTESIAN_POINT ( 'NONE',  ( -28.68588794268872277, 432.8698905683720568, -16.75240474999999307 ) ) ;
#2645 = LINE ( 'NONE', #12274, #5876 ) ;
#2646 = DIRECTION ( 'NONE',  ( -0.000000000000000000, -0.000000000000000000, -1.000000000000000000 ) ) ;
#2647 = CARTESIAN_POINT ( 'NONE',  ( -38.17536295476246977, 472.3073905683720568, -14.20200298773971426 ) ) ;
#2648 = ORIENTED_EDGE ( 'NONE', *, *, #14352, .F. ) ;
#2649 = CARTESIAN_POINT ( 'NONE',  ( -11.93348319268873325, 458.8698905683720000, -2.051577885510841163E-15 ) ) ;
#2650 = CARTESIAN_POINT ( 'NONE',  ( 51.50493485826542894, 160.1716627696692683, 61.61851857202071869 ) ) ;
#2651 = CARTESIAN_POINT ( 'NONE',  ( -47.16347859291445133, 411.3698905765656377, -7.653668647301793193 ) ) ;
#2652 = CARTESIAN_POINT ( 'NONE',  ( 0.000000000000000000, 326.0737056351150613, -33.59072564020503648 ) ) ;
#2653 = CARTESIAN_POINT ( 'NONE',  ( 118.4271928232701043, -343.0245277843623057, 40.00000000000000000 ) ) ;
#2654 = CARTESIAN_POINT ( 'NONE',  ( -8.685887942688642838, 437.3073905765655809, -3.978247347592952732 ) ) ;
#2655 = CARTESIAN_POINT ( 'NONE',  ( -48.68588794268882936, 482.3073905765655240, 3.978247347592901217 ) ) ;
#2656 = CIRCLE ( 'NONE', #4033, 9.999999999999994671 ) ;
#2657 = DIRECTION ( 'NONE',  ( -0.000000000000000000, -0.000000000000000000, -1.000000000000000000 ) ) ;
#2658 = DIRECTION ( 'NONE',  ( 1.191790137725560488E-16, -1.000000000000000000, -0.000000000000000000 ) ) ;
#2659 = CARTESIAN_POINT ( 'NONE',  ( -42.82802356641964536, 248.4948905601784759, 14.14213562373094923 ) ) ;
#2660 = VECTOR ( 'NONE', #2769, 1000.000000000000000 ) ;
#2661 = CARTESIAN_POINT ( 'NONE',  ( -8.685887942688735208, 476.9948905765656377, -2.449293598294705724E-15 ) ) ;
#2662 = CARTESIAN_POINT ( 'NONE',  ( -22.27502019258949417, 432.2448905683720000, -15.47720386886985544 ) ) ;
#2663 = DIRECTION ( 'NONE',  ( 0.000000000000000000, 0.000000000000000000, 1.000000000000000000 ) ) ;
#2664 = CARTESIAN_POINT ( 'NONE',  ( -14.48388495494898542, 259.4323905683720000, 9.489475012073732785 ) ) ;
#2665 = ORIENTED_EDGE ( 'NONE', *, *, #635, .T. ) ;
#2666 = ORIENTED_EDGE ( 'NONE', *, *, #16431, .F. ) ;
#2667 = FACE_OUTER_BOUND ( 'NONE', #17699, .T. ) ;
#2668 = EDGE_LOOP ( 'NONE', ( #11517, #43, #4733, #6560 ) ) ;
#2669 = CARTESIAN_POINT ( 'NONE',  ( -25.35362745456400546, 482.5573905683720000, -16.75240474999999307 ) ) ;
#2670 = EDGE_CURVE ( 'NONE', #7489, #7633, #12316, .T. ) ;
#2671 = VECTOR ( 'NONE', #12923, 1000.000000000000000 ) ;
#2672 = ORIENTED_EDGE ( 'NONE', *, *, #10059, .T. ) ;
#2673 = CARTESIAN_POINT ( 'NONE',  ( -14.54375231895778775, 525.7448905765655809, 14.14213562373094568 ) ) ;
#2674 = CARTESIAN_POINT ( 'NONE',  ( -14.48388495494898365, 237.9323905683720000, 9.489475012073732785 ) ) ;
#2675 = VERTEX_POINT ( 'NONE', #20431 ) ;
#2676 = CARTESIAN_POINT ( 'NONE',  ( -14.48388495494901740, 519.8073905683719431, -9.489475012073734561 ) ) ;
#2677 = DIRECTION ( 'NONE',  ( 0.000000000000000000, 1.000000000000000000, -0.000000000000000000 ) ) ;
#2678 = CIRCLE ( 'NONE', #14773, 10.00000000000000888 ) ;
#2679 = CARTESIAN_POINT ( 'NONE',  ( -10.20829729246299777, 457.6198905765656377, -7.653668647301794969 ) ) ;
#2680 = CARTESIAN_POINT ( 'NONE',  ( -48.68588794268887199, 347.5573905601784190, 3.978247347592742678 ) ) ;
#2681 = ADVANCED_FACE ( 'NONE', ( #12424 ), #17086, .T. ) ;
#2682 = CARTESIAN_POINT ( 'NONE',  ( 0.5805565836007715586, -7.505553499465150935, -4.964436717930768604E-16 ) ) ;
#2683 = CARTESIAN_POINT ( 'NONE',  ( -17.35679799567830628, 453.8073905601784759, -16.95518130045146421 ) ) ;
#2684 = CARTESIAN_POINT ( 'NONE',  ( -11.93348319268870483, 230.3698905683720284, -2.051577885510841163E-15 ) ) ;
#2685 = CARTESIAN_POINT ( 'NONE',  ( -32.01814843081346851, 507.5573905683720568, 16.75240474999999307 ) ) ;
#2686 = CARTESIAN_POINT ( 'NONE',  ( 30.42502041961813575, 271.1055109169419097, -20.00000000000000355 ) ) ;
#2687 = CARTESIAN_POINT ( 'NONE',  ( -14.48388495494898365, 229.8073905683720000, -9.489475012073736337 ) ) ;
#2688 = CARTESIAN_POINT ( 'NONE',  ( -40.53162694259543741, 336.6198905683720000, 11.84573899990672885 ) ) ;
#2689 = VECTOR ( 'NONE', #17263, 1000.000000000000000 ) ;
#2690 = DIRECTION ( 'NONE',  ( 1.000000000000000000, 0.000000000000000000, -0.000000000000000000 ) ) ;
#2691 = CARTESIAN_POINT ( 'NONE',  ( -32.66413529028186247, 274.1823905765656377, 19.99999999999999289 ) ) ;
#2692 = EDGE_CURVE ( 'NONE', #12017, #6673, #15467, .T. ) ;
#2693 = CIRCLE ( 'NONE', #15825, 5.000000000000004441 ) ;
#2694 = CARTESIAN_POINT ( 'NONE',  ( -19.19641293061498644, 377.3073905683720568, 14.20200298773971426 ) ) ;
#2695 = CARTESIAN_POINT ( 'NONE',  ( -36.33955658999050797, 323.8698905765656377, 18.47759065022572500 ) ) ;
#2696 = AXIS2_PLACEMENT_3D ( 'NONE', #6582, #19360, #4651 ) ;
#2697 =( BOUNDED_CURVE ( )  B_SPLINE_CURVE ( 2, ( #12849, #9696, #17711, #7959, #6134, #4725, #3007, #21274, #1386, #16209, #11107, #6446, #19333, #16421, #21173, #4828, #7857 ),
 .UNSPECIFIED., .F., .T. ) 
 B_SPLINE_CURVE_WITH_KNOTS ( ( 3, 2, 2, 2, 2, 2, 2, 2, 3 ),
 ( 0.2812500000000000555, 0.2832031250000000555, 0.2851562500000000555, 0.2871093750000000555, 0.2890625000000001110, 0.2910156250000001110, 0.2929687500000001110, 0.2949218750000001110, 0.2968750000000001110 ),
 .UNSPECIFIED. ) 
 CURVE ( )  GEOMETRIC_REPRESENTATION_ITEM ( )  RATIONAL_B_SPLINE_CURVE ( ( 0.9999999999999994449, 0.9807852804032309857, 1.000000000000000000, 0.9807852804032304306, 1.000000000000000000, 0.9807852804032304306, 1.000000000000000000, 0.9807852804032304306, 1.000000000000000000, 0.9807852804032304306, 1.000000000000000000, 0.9807852804032304306, 1.000000000000000000, 0.9807852804032304306, 1.000000000000000000, 0.9807852804032293204, 1.000000000000001110 ) ) 
 REPRESENTATION_ITEM ( '' )  );
#2698 = CARTESIAN_POINT ( 'NONE',  ( -32.66413529028187668, 389.4323905601784759, 19.99999999999999289 ) ) ;
#2699 = EDGE_CURVE ( 'NONE', #7041, #6110, #186, .T. ) ;
#2700 = CARTESIAN_POINT ( 'NONE',  ( -28.68588794268872277, 378.8848358243226357, 38.00000000000000000 ) ) ;
#2701 = ORIENTED_EDGE ( 'NONE', *, *, #7215, .F. ) ;
#2702 = VERTEX_POINT ( 'NONE', #8943 ) ;
#2703 = CARTESIAN_POINT ( 'NONE',  ( -32.01814843081346851, 513.1823905683720568, -16.75240474999999307 ) ) ;
#2704 = DIRECTION ( 'NONE',  ( -1.000000000000000000, 0.000000000000000000, -0.000000000000000000 ) ) ;
#2705 = ORIENTED_EDGE ( 'NONE', *, *, #13259, .F. ) ;
#2706 = CARTESIAN_POINT ( 'NONE',  ( -32.01814843081344009, 313.1823905683720000, -16.75240474999999307 ) ) ;
#2707 = ORIENTED_EDGE ( 'NONE', *, *, #19267, .F. ) ;
#2708 = CARTESIAN_POINT ( 'NONE',  ( -11.93348319268871727, 328.8698905683720000, -2.051577885510841163E-15 ) ) ;
#2709 = CARTESIAN_POINT ( 'NONE',  ( -42.88789093042843348, 354.8073905683720568, 9.489475012073734561 ) ) ;
#2710 = CARTESIAN_POINT ( 'NONE',  ( -45.64106924314017988, 271.0573905765656946, -11.32908994701042715 ) ) ;
#2711 = CARTESIAN_POINT ( 'NONE',  ( -48.68588794268873698, 573.2448905601785327, 0.000000000000000000 ) ) ;
#2712 = CARTESIAN_POINT ( 'NONE',  ( -44.16309181155855867, 243.2448905683720000, -6.410867750099231266 ) ) ;
#2713 = CARTESIAN_POINT ( 'NONE',  ( -40.01497788969912506, 225.6823905601784759, -16.95518130045146421 ) ) ;
#2714 = CARTESIAN_POINT ( 'NONE',  ( -25.35362745456398414, 398.1823905683720568, 16.75240474999998952 ) ) ;
#2715 = ADVANCED_FACE ( 'NONE', ( #14269 ), #20958, .F. ) ;
#2716 = DIRECTION ( 'NONE',  ( -0.8090169943749473402, 0.000000000000000000, 0.5877852522924733591 ) ) ;
#2717 = LINE ( 'NONE', #3031, #3822 ) ;
#2718 = DIRECTION ( 'NONE',  ( 0.000000000000000000, -1.000000000000000000, 0.000000000000000000 ) ) ;
#2719 = AXIS2_PLACEMENT_3D ( 'NONE', #7627, #20840, #6012 ) ;
#2720 = CARTESIAN_POINT ( 'NONE',  ( -19.19641293061499354, 440.4323905683720000, -14.20200298773971603 ) ) ;
#2721 = VERTEX_POINT ( 'NONE', #751 ) ;
#2722 = CARTESIAN_POINT ( 'NONE',  ( -14.54375231895777709, 450.9948905601784759, 14.14213562373094568 ) ) ;
#2723 = EDGE_CURVE ( 'NONE', #11194, #15706, #13945, .T. ) ;
#2724 = ORIENTED_EDGE ( 'NONE', *, *, #7962, .T. ) ;
#2725 = AXIS2_PLACEMENT_3D ( 'NONE', #1630, #2826, #14619 ) ;
#2726 = ORIENTED_EDGE ( 'NONE', *, *, #2353, .F. ) ;
#2727 = LINE ( 'NONE', #21210, #17359 ) ;
#2728 = CARTESIAN_POINT ( 'NONE',  ( -11.73070664223724791, 333.1823905601784190, -11.32908994701042715 ) ) ;
#2729 = CARTESIAN_POINT ( 'NONE',  ( -45.43829269268871229, 365.6823905683720568, 3.332260488124734632 ) ) ;
#2730 = DIRECTION ( 'NONE',  ( 0.000000000000000000, -0.5000000000000007772, 0.8660254037844381525 ) ) ;
#2731 = CARTESIAN_POINT ( 'NONE',  ( -11.73070664223726745, 497.9323905765655809, -11.32908994701042715 ) ) ;
#2732 = CARTESIAN_POINT ( 'NONE',  ( -35.09675569278794427, 381.9948905683720568, -15.47720386886985544 ) ) ;
#2733 = CARTESIAN_POINT ( 'NONE',  ( -40.53162694259542320, 244.1198905683720284, -11.84573899990672707 ) ) ;
#2734 = CARTESIAN_POINT ( 'NONE',  ( -22.27502019258947996, 396.9948905683720568, 15.47720386886985189 ) ) ;
#2735 = AXIS2_PLACEMENT_3D ( 'NONE', #16601, #11388, #7923 ) ;
#2736 = CARTESIAN_POINT ( 'NONE',  ( -21.03221929538690560, 335.1198905765655809, 18.47759065022572500 ) ) ;
#2737 = CARTESIAN_POINT ( 'NONE',  ( -28.68588794268872633, 174.3162933293988033, 0.000000000000000000 ) ) ;
#2738 = CARTESIAN_POINT ( 'NONE',  ( -11.93348319268871549, 309.1823905683720000, -3.332260488124732856 ) ) ;
#2739 = CARTESIAN_POINT ( 'NONE',  ( -40.53162694259545162, 454.1198905683720568, -11.84573899990672707 ) ) ;
#2740 = CARTESIAN_POINT ( 'NONE',  ( -24.70764059509555821, 460.0573905601785327, 19.99999999999998934 ) ) ;
#2741 = CARTESIAN_POINT ( 'NONE',  ( 2.416697501590669095, 172.9933428177121471, 49.99999999999999289 ) ) ;
#2742 = DIRECTION ( 'NONE',  ( 0.000000000000000000, -0.9253149302858357794, -0.3791995250394160633 ) ) ;
#2743 = CARTESIAN_POINT ( 'NONE',  ( -14.48388495494899786, 359.4323905683719431, 9.489475012073732785 ) ) ;
#2744 = CARTESIAN_POINT ( 'NONE',  ( -25.35362745456400901, 501.0573905683720568, -16.75240474999999307 ) ) ;
#2745 = CARTESIAN_POINT ( 'NONE',  ( -8.685887942688740537, 512.5573905601785327, -3.978247347593165895 ) ) ;
#2746 = CARTESIAN_POINT ( 'NONE',  ( -38.17536295476245556, 332.3073905683720000, -14.20200298773971426 ) ) ;
#2747 = CONICAL_SURFACE ( 'NONE', #5493, 3.309499999999999886, 0.7853981633974407295 ) ;
#2748 = ORIENTED_EDGE ( 'NONE', *, *, #6180, .T. ) ;
#2749 = CARTESIAN_POINT ( 'NONE',  ( -40.01497788969916058, 525.6823905601785327, -16.95518130045146421 ) ) ;
#2750 = EDGE_LOOP ( 'NONE', ( #15105, #18089, #11435, #2248 ) ) ;
#2751 = ADVANCED_BREP_SHAPE_REPRESENTATION ( '', ( #19141, #12794 ), #718 ) ;
#2752 = EDGE_CURVE ( 'NONE', #349, #8848, #3971, .T. ) ;
#2753 = DIRECTION ( 'NONE',  ( 1.000000000000000000, 0.000000000000000000, 0.000000000000000000 ) ) ;
#2754 = EDGE_CURVE ( 'NONE', #10000, #13614, #15997, .T. ) ;
#2755 = CARTESIAN_POINT ( 'NONE',  ( -40.53162694259544452, 416.6198905683720000, 11.84573899990672885 ) ) ;
#2756 = CARTESIAN_POINT ( 'NONE',  ( 151.4788465195079823, 620.7448905601785327, -8.917803138848077182 ) ) ;
#2757 = LINE ( 'NONE', #2969, #20753 ) ;
#2758 = CARTESIAN_POINT ( 'NONE',  ( -40.53162694259545162, 472.6198905683720000, -11.84573899990672707 ) ) ;
#2759 = ORIENTED_EDGE ( 'NONE', *, *, #20663, .F. ) ;
#2760 = CARTESIAN_POINT ( 'NONE',  ( -45.43829269268872650, 464.1823905683720000, 3.332260488124734632 ) ) ;
#2761 = DIRECTION ( 'NONE',  ( 1.000000000000000000, 0.000000000000000000, 0.000000000000000000 ) ) ;
#2762 = FACE_OUTER_BOUND ( 'NONE', #12670, .T. ) ;
#2763 = CARTESIAN_POINT ( 'NONE',  ( -10.20829729246299067, 397.6198905765655809, -7.653668647301794969 ) ) ;
#2764 = CARTESIAN_POINT ( 'NONE',  ( 158.8141120573112630, 620.7448905601785327, 4.999999999999990230 ) ) ;
#2765 = DIRECTION ( 'NONE',  ( -1.191790137725560488E-16, 1.000000000000000000, -0.000000000000000000 ) ) ;
#2766 = DIRECTION ( 'NONE',  ( 0.000000000000000000, 0.000000000000000000, -1.000000000000000000 ) ) ;
#2767 = CARTESIAN_POINT ( 'NONE',  ( -10.20829729246297468, 256.3698905765656377, 7.653668647301790529 ) ) ;
#2768 = AXIS2_PLACEMENT_3D ( 'NONE', #3557, #8303, #10033 ) ;
#2769 = DIRECTION ( 'NONE',  ( -1.374938938973709817E-16, 1.000000000000000000, 0.000000000000000000 ) ) ;
#2770 = CARTESIAN_POINT ( 'NONE',  ( 125.7989814974898053, 10.52886280891152104, 40.00000000000000000 ) ) ;
#2771 = CARTESIAN_POINT ( 'NONE',  ( -45.43280446313950449, 223.9102039777116602, 0.4287796227366179602 ) ) ;
#2772 = CARTESIAN_POINT ( 'NONE',  ( -8.685887942688708563, 241.9323905601784475, 3.978247347593161010 ) ) ;
#2773 = DIRECTION ( 'NONE',  ( 1.000000000000000000, 0.000000000000000000, 0.000000000000000000 ) ) ;
#2774 = CARTESIAN_POINT ( 'NONE',  ( -45.43829269268871940, 425.3698905683720568, 0.000000000000000000 ) ) ;
#2775 = CARTESIAN_POINT ( 'NONE',  ( 105.7989814974898479, 142.5259582928263455, -20.00000000000000355 ) ) ;
#2776 = CARTESIAN_POINT ( 'NONE',  ( -13.20868407381884779, 259.7448905683720000, 6.410867750099229490 ) ) ;
#2777 = EDGE_LOOP ( 'NONE', ( #19575, #2592, #4506, #5910 ) ) ;
#2778 = ORIENTED_EDGE ( 'NONE', *, *, #3803, .T. ) ;
#2779 = ORIENTED_EDGE ( 'NONE', *, *, #7166, .T. ) ;
#2780 = CARTESIAN_POINT ( 'NONE',  ( -22.27502019258948707, 458.4948905683720568, 15.47720386886985189 ) ) ;
#2781 = CARTESIAN_POINT ( 'NONE',  ( -40.01497788969912506, 230.4323905765656377, -16.95518130045146421 ) ) ;
#2782 = EDGE_LOOP ( 'NONE', ( #14261, #6010, #20550, #14725, #8206, #13930, #5554, #2865 ) ) ;
#2783 = CARTESIAN_POINT ( 'NONE',  ( -10.20829729246298534, 362.8698905601784759, -7.653668647301794969 ) ) ;
#2784 = CARTESIAN_POINT ( 'NONE',  ( -40.53162694259542320, 232.6198905683720000, -11.84573899990672707 ) ) ;
#2785 = VERTEX_POINT ( 'NONE', #7532 ) ;
#2786 = CARTESIAN_POINT ( 'NONE',  ( -19.19641293061500420, 520.4323905683719431, -14.20200298773971603 ) ) ;
#2787 = DIRECTION ( 'NONE',  ( -1.000000000000000000, -0.000000000000000000, -0.000000000000000000 ) ) ;
#2788 = CARTESIAN_POINT ( 'NONE',  ( -36.33955658999052929, 463.8698905765656377, 18.47759065022572500 ) ) ;
#2789 = FACE_OUTER_BOUND ( 'NONE', #11656, .T. ) ;
#2790 = CARTESIAN_POINT ( 'NONE',  ( -17.35679799567828141, 285.4323905765656377, 16.95518130045146421 ) ) ;
#2791 = VECTOR ( 'NONE', #17043, 999.9999999999998863 ) ;
#2792 = FACE_BOUND ( 'NONE', #3520, .T. ) ;
#2793 = CARTESIAN_POINT ( 'NONE',  ( -44.16309181155855867, 224.7448905683720568, -6.410867750099231266 ) ) ;
#2794 = PLANE ( 'NONE',  #5248 ) ;
#2795 = CARTESIAN_POINT ( 'NONE',  ( -11.93348319268870661, 229.1823905683720284, -3.332260488124732856 ) ) ;
#2796 = CARTESIAN_POINT ( 'NONE',  ( -28.68588794268870856, 327.8698905683720000, 16.75240474999999307 ) ) ;
#2797 = CARTESIAN_POINT ( 'NONE',  ( -8.685887942688717445, 322.2448905601784759, -2.449293598294705724E-15 ) ) ;
#2798 = CARTESIAN_POINT ( 'NONE',  ( 0.2595206531159287011, 2.531175536751830268, 6.500000000000000888 ) ) ;
#2799 = CARTESIAN_POINT ( 'NONE',  ( -45.43829269268869808, 315.6823905683720000, 3.332260488124734632 ) ) ;
#2800 = CARTESIAN_POINT ( 'NONE',  ( -19.19641293061498644, 387.3073905683720000, 14.20200298773971426 ) ) ;
#2801 = VECTOR ( 'NONE', #12791, 999.9999999999998863 ) ;
#2802 = EDGE_CURVE ( 'NONE', #12320, #1316, #19007, .T. ) ;
#2803 = CARTESIAN_POINT ( 'NONE',  ( -35.09675569278796559, 533.4948905683720568, -15.47720386886985544 ) ) ;
#2804 = VECTOR ( 'NONE', #17124, 1000.000000000000000 ) ;
#2805 = CARTESIAN_POINT ( 'NONE',  ( -21.03221929538692692, 384.1198905601784759, -18.47759065022572855 ) ) ;
#2806 = DIRECTION ( 'NONE',  ( 1.000000000000000000, 0.000000000000000000, 0.000000000000000000 ) ) ;
#2807 = ORIENTED_EDGE ( 'NONE', *, *, #13252, .T. ) ;
#2808 = VERTEX_POINT ( 'NONE', #19226 ) ;
#2809 = CARTESIAN_POINT ( 'NONE',  ( -22.27502019258950128, 492.2448905683720000, -15.47720386886985544 ) ) ;
#2810 = LINE ( 'NONE', #19027, #18368 ) ;
#2811 = EDGE_LOOP ( 'NONE', ( #2591, #8808, #16191, #16987 ) ) ;
#2812 = CARTESIAN_POINT ( 'NONE',  ( -45.43829269268870519, 295.3698905683720568, 0.000000000000000000 ) ) ;
#2813 = AXIS2_PLACEMENT_3D ( 'NONE', #8027, #1787, #5117 ) ;
#2814 = CARTESIAN_POINT ( 'NONE',  ( -22.27502019258948351, 330.7448905683720568, -15.47720386886985544 ) ) ;
#2815 = MECHANICAL_DESIGN_GEOMETRIC_PRESENTATION_REPRESENTATION (  '', ( #9005 ), #17309 ) ;
#2816 = CARTESIAN_POINT ( 'NONE',  ( -10.20829729246297646, 266.3698905765656377, 7.653668647301790529 ) ) ;
#2817 = CYLINDRICAL_SURFACE ( 'NONE', #13121, 19.99999999999999645 ) ;
#2818 = CARTESIAN_POINT ( 'NONE',  ( -71.26501780185373036, 135.1716627696692683, -25.00000000000000000 ) ) ;
#2819 = CARTESIAN_POINT ( 'NONE',  ( -14.48388495494900141, 389.4323905683720568, 9.489475012073732785 ) ) ;
#2820 = EDGE_CURVE ( 'NONE', #14497, #20490, #3928, .T. ) ;
#2821 = CARTESIAN_POINT ( 'NONE',  ( -48.68588794268871567, 447.2448905601785327, 0.000000000000000000 ) ) ;
#2822 = FACE_OUTER_BOUND ( 'NONE', #16266, .T. ) ;
#2823 =( BOUNDED_CURVE ( )  B_SPLINE_CURVE ( 2, ( #17250, #20815, #15741, #9014, #14016, #15529, #19080, #18966, #10953, #2327, #12596, #4263, #15847, #5768, #15952, #5665, #14228 ),
 .UNSPECIFIED., .F., .T. ) 
 B_SPLINE_CURVE_WITH_KNOTS ( ( 3, 2, 2, 2, 2, 2, 2, 2, 3 ),
 ( 0.6718750000000002220, 0.6738281250000002220, 0.6757812500000002220, 0.6777343750000002220, 0.6796875000000002220, 0.6816406250000002220, 0.6835937500000002220, 0.6855468750000002220, 0.6875000000000002220 ),
 .UNSPECIFIED. ) 
 CURVE ( )  GEOMETRIC_REPRESENTATION_ITEM ( )  RATIONAL_B_SPLINE_CURVE ( ( 0.9999999999999977796, 0.9807852804032326510, 1.000000000000000000, 0.9807852804032304306, 1.000000000000000000, 0.9807852804032304306, 1.000000000000000000, 0.9807852804032304306, 1.000000000000000000, 0.9807852804032304306, 1.000000000000000000, 0.9807852804032304306, 1.000000000000000000, 0.9807852804032304306, 1.000000000000000000, 0.9807852804032282101, 1.000000000000002220 ) ) 
 REPRESENTATION_ITEM ( '' )  );
#2824 = DIRECTION ( 'NONE',  ( 0.000000000000000000, 0.000000000000000000, -1.000000000000000000 ) ) ;
#2825 = CARTESIAN_POINT ( 'NONE',  ( -45.43829269268871229, 443.5573905683720000, -3.332260488124726194 ) ) ;
#2826 = DIRECTION ( 'NONE',  ( -1.191790137725560488E-16, 1.000000000000000000, -0.000000000000000000 ) ) ;
#2827 = ORIENTED_EDGE ( 'NONE', *, *, #10142, .F. ) ;
#2828 = CARTESIAN_POINT ( 'NONE',  ( -40.01497788969913927, 448.8073905601785327, 16.95518130045146776 ) ) ;
#2829 = VERTEX_POINT ( 'NONE', #9157 ) ;
#2830 = ORIENTED_EDGE ( 'NONE', *, *, #16657, .F. ) ;
#2831 = ORIENTED_EDGE ( 'NONE', *, *, #1697, .F. ) ;
#2832 = FACE_OUTER_BOUND ( 'NONE', #2750, .T. ) ;
#2833 = AXIS2_PLACEMENT_3D ( 'NONE', #6354, #1396, #4837 ) ;
#2834 = CARTESIAN_POINT ( 'NONE',  ( -14.54375231895776110, 320.9948905601784759, 14.14213562373094568 ) ) ;
#2835 = CARTESIAN_POINT ( 'NONE',  ( 91.21585410611801592, 31.85652257517428865, -85.46735025547123143 ) ) ;
#2836 = EDGE_CURVE ( 'NONE', #5613, #21078, #16037, .T. ) ;
#2837 = CARTESIAN_POINT ( 'NONE',  ( -40.53162694259543741, 356.6198905683720000, 11.84573899990672885 ) ) ;
#2838 = DIRECTION ( 'NONE',  ( 1.191790137725560488E-16, -1.000000000000000000, 0.000000000000000000 ) ) ;
#2839 = CARTESIAN_POINT ( 'NONE',  ( -40.01497788969916058, 510.4323905765656946, -16.95518130045146421 ) ) ;
#2840 = CARTESIAN_POINT ( 'NONE',  ( -16.84014894278199392, 380.1198905683720568, -11.84573899990672707 ) ) ;
#2841 = DIRECTION ( 'NONE',  ( 1.191790137725560488E-16, -1.000000000000000000, 0.000000000000000000 ) ) ;
#2842 = CARTESIAN_POINT ( 'NONE',  ( -44.16309181155857289, 414.4948905683720000, 6.410867750099241924 ) ) ;
#2843 = CARTESIAN_POINT ( 'NONE',  ( -47.16347859291444422, 332.6198905765656377, 7.653668647301805628 ) ) ;
#2844 = CARTESIAN_POINT ( 'NONE',  ( -10.20829729246298001, 322.8698905601784759, -7.653668647301794969 ) ) ;
#2845 = CARTESIAN_POINT ( 'NONE',  ( -14.48388495494899253, 299.8073905683719431, -9.489475012073734561 ) ) ;
#2846 = CARTESIAN_POINT ( 'NONE',  ( -19.19641293061498999, 458.8073905683720000, 14.20200298773971426 ) ) ;
#2847 = EDGE_CURVE ( 'NONE', #21308, #18480, #18777, .T. ) ;
#2848 = CARTESIAN_POINT ( 'NONE',  ( -8.685887942688733432, 462.2448905601784759, -2.449293598294705724E-15 ) ) ;
#2849 = CARTESIAN_POINT ( 'NONE',  ( 0.01372220897661660666, 5.948365447239580384, 2.697128823393879493 ) ) ;
#2850 = PLANE ( 'NONE',  #15774 ) ;
#2851 = AXIS2_PLACEMENT_3D ( 'NONE', #10011, #18238, #200 ) ;
#2852 = CARTESIAN_POINT ( 'NONE',  ( -44.16309181155856578, 375.9948905683720568, 6.410867750099241924 ) ) ;
#2853 = CARTESIAN_POINT ( 'NONE',  ( -38.17536295476246977, 505.4323905683720568, 14.20200298773971781 ) ) ;
#2854 = CARTESIAN_POINT ( 'NONE',  ( -8.685887942688738761, 502.2448905601784190, -2.449293598294705724E-15 ) ) ;
#2855 = CARTESIAN_POINT ( 'NONE',  ( -14.48388495494899431, 319.8073905683720568, -9.489475012073736337 ) ) ;
#2856 = ORIENTED_EDGE ( 'NONE', *, *, #17543, .F. ) ;
#2857 = CARTESIAN_POINT ( 'NONE',  ( -48.68588794268869435, 257.2448905601784759, 0.000000000000000000 ) ) ;
#2858 = VERTEX_POINT ( 'NONE', #1595 ) ;
#2859 = VECTOR ( 'NONE', #18979, 1000.000000000000114 ) ;
#2860 = FACE_OUTER_BOUND ( 'NONE', #2326, .T. ) ;
#2861 = CARTESIAN_POINT ( 'NONE',  ( -25.35362745456398770, 428.1823905683720568, 16.75240474999998952 ) ) ;
#2862 = DIRECTION ( 'NONE',  ( -1.000000000000000000, 0.000000000000000000, 0.000000000000000000 ) ) ;
#2863 = SURFACE_SIDE_STYLE ('',( #14544 ) ) ;
#2864 = CARTESIAN_POINT ( 'NONE',  ( -22.27502019258948707, 446.9948905683720000, 15.47720386886985189 ) ) ;
#2865 = ORIENTED_EDGE ( 'NONE', *, *, #8030, .T. ) ;
#2866 = CARTESIAN_POINT ( 'NONE',  ( -13.20868407381887089, 458.2448905683720568, 6.410867750099229490 ) ) ;
#2867 = DIRECTION ( 'NONE',  ( 1.000000000000000000, 0.000000000000000000, 0.000000000000000000 ) ) ;
#2868 = CARTESIAN_POINT ( 'NONE',  ( -36.33955658999051508, 415.3698905601784759, -18.47759065022572855 ) ) ;
#2869 = CARTESIAN_POINT ( 'NONE',  ( -47.16347859291444422, 382.6198905765655809, 7.653668647301805628 ) ) ;
#2870 = DIRECTION ( 'NONE',  ( -0.000000000000000000, 1.000000000000000000, -0.000000000000000000 ) ) ;
#2871 = CARTESIAN_POINT ( 'NONE',  ( -13.68588794268869790, 223.9102039777116602, 1.836970198721029589E-15 ) ) ;
#2872 = CARTESIAN_POINT ( 'NONE',  ( -28.68588794268874054, 573.2448905601785327, 0.000000000000000000 ) ) ;
#2873 = PLANE ( 'NONE',  #20135 ) ;
#2874 = CARTESIAN_POINT ( 'NONE',  ( -48.68588794268870856, 337.2448905601784759, 0.000000000000000000 ) ) ;
#2875 = DIRECTION ( 'NONE',  ( -1.000000000000000000, 0.000000000000000000, 0.000000000000000000 ) ) ;
#2876 = DIRECTION ( 'NONE',  ( -1.191790137725560488E-16, 1.000000000000000000, -0.000000000000000000 ) ) ;
#2877 = ADVANCED_FACE ( 'NONE', ( #4515 ), #14584, .F. ) ;
#2878 = AXIS2_PLACEMENT_3D ( 'NONE', #12735, #19327, #1174 ) ;
#2879 = CARTESIAN_POINT ( 'NONE',  ( -19.19641293061498999, 418.8073905683720568, 14.20200298773971426 ) ) ;
#2880 = FACE_OUTER_BOUND ( 'NONE', #7918, .T. ) ;
#2881 = CARTESIAN_POINT ( 'NONE',  ( -25.35362745456396638, 258.1823905683720000, 16.75240474999998952 ) ) ;
#2882 = VERTEX_POINT ( 'NONE', #4936 ) ;
#2883 = ORIENTED_EDGE ( 'NONE', *, *, #19354, .T. ) ;
#2884 = DIRECTION ( 'NONE',  ( 1.000000000000000000, 0.000000000000000000, 0.000000000000000000 ) ) ;
#2885 = EDGE_LOOP ( 'NONE', ( #4892, #17666 ) ) ;
#2886 = CARTESIAN_POINT ( 'NONE',  ( -11.93348319268873325, 460.0573905683720568, 3.332260488124728859 ) ) ;
#2887 = CARTESIAN_POINT ( 'NONE',  ( -14.54375231895775400, 228.2448905765656093, -14.14213562373094746 ) ) ;
#2888 = ADVANCED_FACE ( 'NONE', ( #1273 ), #16417, .T. ) ;
#2889 = VECTOR ( 'NONE', #5929, 1000.000000000000000 ) ;
#2890 = ORIENTED_EDGE ( 'NONE', *, *, #21068, .F. ) ;
#2891 = CARTESIAN_POINT ( 'NONE',  ( -42.91697296918459870, 206.7606908932681336, 4.742769269235595608 ) ) ;
#2892 = CARTESIAN_POINT ( 'NONE',  ( -44.16309181155859420, 534.7448905683720568, -6.410867750099231266 ) ) ;
#2893 = EDGE_CURVE ( 'NONE', #18972, #18441, #14274, .T. ) ;
#2894 = AXIS2_PLACEMENT_3D ( 'NONE', #13804, #5570, #20084 ) ;
#2895 = ORIENTED_EDGE ( 'NONE', *, *, #9613, .T. ) ;
#2896 = CARTESIAN_POINT ( 'NONE',  ( 6.416697501590670427, 172.9933428177121471, 60.00000000000000000 ) ) ;
#2897 = CARTESIAN_POINT ( 'NONE',  ( 2.416697501590669095, 172.9933428177121471, 45.00000000000000000 ) ) ;
#2898 = EDGE_CURVE ( 'NONE', #15497, #15607, #6658, .T. ) ;
#2899 = CARTESIAN_POINT ( 'NONE',  ( -8.685887942688735208, 456.6823905765655809, 3.978247347593161010 ) ) ;
#2900 = DIRECTION ( 'NONE',  ( -1.000000000000000000, 0.000000000000000000, 0.000000000000000000 ) ) ;
#2901 = DIRECTION ( 'NONE',  ( -1.000000000000000000, 0.000000000000000000, 0.000000000000000000 ) ) ;
#2902 = CARTESIAN_POINT ( 'NONE',  ( -42.82802356641964536, 240.7448905765656093, -14.14213562373094746 ) ) ;
#2903 = CARTESIAN_POINT ( 'NONE',  ( -28.68588794268870146, 289.7448905601784759, 19.99999999999999289 ) ) ;
#2904 = CARTESIAN_POINT ( 'NONE',  ( -38.17536295476244135, 222.3073905683720284, -14.20200298773971426 ) ) ;
#2905 = CARTESIAN_POINT ( 'NONE',  ( -42.88789093042842637, 316.3073905683720568, 9.489475012073736337 ) ) ;
#2906 = ADVANCED_FACE ( 'NONE', ( #14799 ), #6549, .F. ) ;
#2907 = VECTOR ( 'NONE', #19983, 1000.000000000000000 ) ;
#2908 = DIRECTION ( 'NONE',  ( -0.000000000000000000, -0.000000000000000000, 1.000000000000000000 ) ) ;
#2909 = CARTESIAN_POINT ( 'NONE',  ( -21.03221929538691271, 380.3698905601784759, 18.47759065022572500 ) ) ;
#2910 = VECTOR ( 'NONE', #1085, 1000.000000000000000 ) ;
#2911 = CARTESIAN_POINT ( 'NONE',  ( -45.43829269268869808, 315.0573905683720000, -3.332260488124726194 ) ) ;
#2912 = CARTESIAN_POINT ( 'NONE',  ( -35.09675569278795138, 375.7448905683720000, 15.47720386886985366 ) ) ;
#2913 = CARTESIAN_POINT ( 'NONE',  ( -14.48388495494901740, 521.3073905683720568, -9.489475012073734561 ) ) ;
#2914 = CARTESIAN_POINT ( 'NONE',  ( -11.73070664223724791, 361.3073905601785327, 11.32908994701042005 ) ) ;
#2915 = CARTESIAN_POINT ( 'NONE',  ( 60.03793209889851568, 10.52886280891152104, -136.1729372809869005 ) ) ;
#2916 = ORIENTED_EDGE ( 'NONE', *, *, #20244, .F. ) ;
#2917 = CARTESIAN_POINT ( 'NONE',  ( -19.19641293061499354, 488.8073905683720568, 14.20200298773971426 ) ) ;
#2918 = SURFACE_STYLE_USAGE ( .BOTH. , #14707 ) ;
#2919 = CARTESIAN_POINT ( 'NONE',  ( -45.43829269268870519, 283.8698905683720568, 0.000000000000000000 ) ) ;
#2920 = ORIENTED_EDGE ( 'NONE', *, *, #17887, .F. ) ;
#2921 = CARTESIAN_POINT ( 'NONE',  ( -32.01814843081344009, 287.5573905683720000, 16.75240474999999307 ) ) ;
#2922 = CARTESIAN_POINT ( 'NONE',  ( -13.20868407381885490, 328.2448905683720000, 6.410867750099229490 ) ) ;
#2923 = CARTESIAN_POINT ( 'NONE',  ( -11.73070664223723725, 257.9323905765655809, -11.32908994701042715 ) ) ;
#2924 = CARTESIAN_POINT ( 'NONE',  ( -40.01497788969915348, 475.6823905601784190, -16.95518130045146421 ) ) ;
#2925 = CARTESIAN_POINT ( 'NONE',  ( -13.20868407381884424, 228.2448905683720568, 6.410867750099229490 ) ) ;
#2926 = CARTESIAN_POINT ( 'NONE',  ( -25.35362745456398059, 368.1823905683721136, 16.75240474999998952 ) ) ;
#2927 = CARTESIAN_POINT ( 'NONE',  ( -43.47648769733579854, 200.8087914445877971, 2.512805286998617049 ) ) ;
#2928 = LINE ( 'NONE', #7674, #14204 ) ;
#2929 = CARTESIAN_POINT ( 'NONE',  ( -8.685887942688708563, 252.2448905601784475, -2.449293598294705724E-15 ) ) ;
#2930 = CARTESIAN_POINT ( 'NONE',  ( -22.27502019258948707, 436.9948905683720568, 15.47720386886985189 ) ) ;
#2931 = CARTESIAN_POINT ( 'NONE',  ( 29.72350413846044859, 280.4463447002762564, -40.00000000000000000 ) ) ;
#2932 = ORIENTED_EDGE ( 'NONE', *, *, #1483, .F. ) ;
#2933 = CARTESIAN_POINT ( 'NONE',  ( -32.66413529028188378, 445.0573905601784759, -19.99999999999999289 ) ) ;
#2934 = VERTEX_POINT ( 'NONE', #16203 ) ;
#2935 = ORIENTED_EDGE ( 'NONE', *, *, #7105, .F. ) ;
#2936 = VERTEX_POINT ( 'NONE', #6441 ) ;
#2937 = CARTESIAN_POINT ( 'NONE',  ( -28.68588794268871212, 354.4948905765656377, 19.99999999999999289 ) ) ;
#2938 = CARTESIAN_POINT ( 'NONE',  ( -45.64106924314017988, 328.1823905601784759, 11.32908994701042715 ) ) ;
#2939 = DIRECTION ( 'NONE',  ( -0.7071067811865511255, 8.659560562354889717E-17, -0.7071067811865440200 ) ) ;
#2940 = EDGE_CURVE ( 'NONE', #9142, #15603, #7954, .T. ) ;
#2941 = CARTESIAN_POINT ( 'NONE',  ( -19.19641293061498288, 351.9323905683720568, -14.20200298773971603 ) ) ;
#2942 = DIRECTION ( 'NONE',  ( 1.000000000000000000, 0.000000000000000000, 0.000000000000000000 ) ) ;
#2943 = CARTESIAN_POINT ( 'NONE',  ( -28.68588794268873343, 509.4948905765655809, -19.99999999999999289 ) ) ;
#2944 = CARTESIAN_POINT ( 'NONE',  ( -28.68588794268871567, 386.3698905683720568, 16.75240474999999307 ) ) ;
#2945 = CARTESIAN_POINT ( 'NONE',  ( -42.88789093042841927, 226.3073905683720000, 9.489475012073736337 ) ) ;
#2946 = CARTESIAN_POINT ( 'NONE',  ( -22.27502019258949062, 390.7448905683720000, -15.47720386886985544 ) ) ;
#2947 = CARTESIAN_POINT ( 'NONE',  ( -21.03221929538691981, 318.8698905765656377, -18.47759065022572855 ) ) ;
#2948 = CARTESIAN_POINT ( 'NONE',  ( -42.82802356641966668, 425.9948905601784759, -14.14213562373094746 ) ) ;
#2949 = CARTESIAN_POINT ( 'NONE',  ( -13.20868407381885135, 279.4948905683720000, -6.410867750099233042 ) ) ;
#2950 =( BOUNDED_CURVE ( )  B_SPLINE_CURVE ( 2, ( #16937, #8379, #7070, #15003, #293, #13591, #15212, #18332, #3522, #6756, #13374, #10210, #10109, #13690, #3834, #18541, #20282 ),
 .UNSPECIFIED., .F., .T. ) 
 B_SPLINE_CURVE_WITH_KNOTS ( ( 3, 2, 2, 2, 2, 2, 2, 2, 3 ),
 ( 0.000000000000000000, 0.001953125000000046838, 0.003906250000000093675, 0.005859375000000140513, 0.007812500000000187350, 0.009765625000000234188, 0.01171875000000028103, 0.01367187500000032786, 0.01562500000000037470 ),
 .UNSPECIFIED. ) 
 CURVE ( )  GEOMETRIC_REPRESENTATION_ITEM ( )  RATIONAL_B_SPLINE_CURVE ( ( 1.000000000000000000, 0.9807852804032304306, 1.000000000000000000, 0.9807852804032304306, 1.000000000000000000, 0.9807852804032304306, 1.000000000000000000, 0.9807852804032304306, 1.000000000000000000, 0.9807852804032304306, 1.000000000000000000, 0.9807852804032304306, 1.000000000000000000, 0.9807852804032304306, 1.000000000000000000, 0.9807852804032267668, 1.000000000000003775 ) ) 
 REPRESENTATION_ITEM ( '' )  );
#2951 = CARTESIAN_POINT ( 'NONE',  ( -38.17536295476245556, 436.9323905683720568, 14.20200298773971781 ) ) ;
#2952 = AXIS2_PLACEMENT_3D ( 'NONE', #3980, #18689, #19020 ) ;
#2953 = DIRECTION ( 'NONE',  ( 1.250996701150283068E-16, -1.000000000000000000, 0.000000000000000000 ) ) ;
#2954 = DIRECTION ( 'NONE',  ( 1.000000000000000000, 0.000000000000000000, 0.000000000000000000 ) ) ;
#2955 = DIRECTION ( 'NONE',  ( 1.000000000000000000, 0.000000000000000000, -0.000000000000000000 ) ) ;
#2956 = ADVANCED_FACE ( 'NONE', ( #7852 ), #6232, .F. ) ;
#2957 = CARTESIAN_POINT ( 'NONE',  ( -40.53162694259543741, 354.1198905683720568, -11.84573899990672707 ) ) ;
#2958 = CARTESIAN_POINT ( 'NONE',  ( -45.43829269268871940, 503.5573905683720000, -3.332260488124726194 ) ) ;
#2959 = CARTESIAN_POINT ( 'NONE',  ( -40.01497788969915348, 505.6823905601784759, -16.95518130045146421 ) ) ;
#2960 = CARTESIAN_POINT ( 'NONE',  ( -32.01814843081344009, 316.0573905683720000, 16.75240474999999307 ) ) ;
#2961 = ORIENTED_EDGE ( 'NONE', *, *, #7094, .F. ) ;
#2962 = CARTESIAN_POINT ( 'NONE',  ( -10.20829729246300488, 522.8698905601785327, -7.653668647301794969 ) ) ;
#2963 = VERTEX_POINT ( 'NONE', #8063 ) ;
#2964 = CARTESIAN_POINT ( 'NONE',  ( 10.41669750159067220, 172.9933428177121471, 45.00000000000000000 ) ) ;
#2965 = DIRECTION ( 'NONE',  ( -0.8865057725575725689, 0.000000000000000000, 0.4627175328665443232 ) ) ;
#2966 = EDGE_CURVE ( 'NONE', #15904, #182, #17911, .T. ) ;
#2967 = CARTESIAN_POINT ( 'NONE',  ( -38.17536295476245556, 416.9323905683720568, 14.20200298773971781 ) ) ;
#2968 = FACE_OUTER_BOUND ( 'NONE', #21263, .T. ) ;
#2969 = CARTESIAN_POINT ( 'NONE',  ( 162.8695233526006803, 620.7448905601785327, -10.81142786866620575 ) ) ;
#2970 = CARTESIAN_POINT ( 'NONE',  ( -40.53162694259544452, 435.1198905683720000, 11.84573899990672885 ) ) ;
#2971 = ORIENTED_EDGE ( 'NONE', *, *, #14654, .T. ) ;
#2972 = CARTESIAN_POINT ( 'NONE',  ( -32.01814843081345430, 476.0573905683720000, 16.75240474999999307 ) ) ;
#2973 = DIRECTION ( 'NONE',  ( 0.000000000000000000, 0.000000000000000000, 1.000000000000000000 ) ) ;
#2974 = CARTESIAN_POINT ( 'NONE',  ( 71.23374292195467206, 79.16544270676152451, 94.99999999999994316 ) ) ;
#2975 = CARTESIAN_POINT ( 'NONE',  ( -8.685887942688724550, 387.3073905765656377, -3.978247347593165895 ) ) ;
#2976 = CARTESIAN_POINT ( 'NONE',  ( -25.61611216564576665, 45.79743936472188182, 49.50645936902517263 ) ) ;
#2977 = CARTESIAN_POINT ( 'NONE',  ( -28.68588794268875475, 600.7448905601785327, 0.000000000000000000 ) ) ;
#2978 = FACE_OUTER_BOUND ( 'NONE', #14370, .T. ) ;
#2979 = LINE ( 'NONE', #1353, #1837 ) ;
#2980 = DIRECTION ( 'NONE',  ( 0.000000000000000000, 1.000000000000000000, 0.000000000000000000 ) ) ;
#2981 = CARTESIAN_POINT ( 'NONE',  ( -14.54375231895775755, 253.4948905601784759, -14.14213562373094746 ) ) ;
#2982 = LINE ( 'NONE', #11079, #9368 ) ;
#2983 = CARTESIAN_POINT ( 'NONE',  ( -32.01814843081345430, 427.5573905683720000, 16.75240474999999307 ) ) ;
#2984 = LINE ( 'NONE', #4699, #1623 ) ;
#2985 = CARTESIAN_POINT ( 'NONE',  ( -38.17536295476243424, 246.9323905683720284, 14.20200298773971781 ) ) ;
#2986 = ORIENTED_EDGE ( 'NONE', *, *, #11157, .F. ) ;
#2987 = CARTESIAN_POINT ( 'NONE',  ( -8.685887942688820473, 426.6823905765655809, 3.978247347593374172 ) ) ;
#2988 = ORIENTED_EDGE ( 'NONE', *, *, #21108, .T. ) ;
#2989 = CARTESIAN_POINT ( 'NONE',  ( -22.27502019258949773, 472.2448905683720568, -15.47720386886985544 ) ) ;
#2990 = CARTESIAN_POINT ( 'NONE',  ( -28.68588794268869790, 219.4948905765656377, -19.99999999999999289 ) ) ;
#2991 = VERTEX_POINT ( 'NONE', #19435 ) ;
#2992 = LINE ( 'NONE', #7941, #3820 ) ;
#2993 = CARTESIAN_POINT ( 'NONE',  ( -13.20868407381888154, 530.9948905683720568, -6.410867750099233042 ) ) ;
#2994 = ORIENTED_EDGE ( 'NONE', *, *, #19444, .T. ) ;
#2995 = CARTESIAN_POINT ( 'NONE',  ( -42.88789093042845479, 522.9323905683720568, -9.489475012073734561 ) ) ;
#2996 = CARTESIAN_POINT ( 'NONE',  ( -5.085585815314819236E-15, 5.948846446048898784, -2.696295709017757503 ) ) ;
#2997 = VECTOR ( 'NONE', #21329, 1000.000000000000000 ) ;
#2998 = CARTESIAN_POINT ( 'NONE',  ( -32.66413529028188378, 444.1823905765655809, 19.99999999999999289 ) ) ;
#2999 = CARTESIAN_POINT ( 'NONE',  ( -48.68588794268870856, 347.2448905601784759, 0.000000000000000000 ) ) ;
#3000 = DIRECTION ( 'NONE',  ( -1.191790137725560488E-16, 1.000000000000000000, -0.000000000000000000 ) ) ;
#3001 = CARTESIAN_POINT ( 'NONE',  ( -49.57497958038186425, 230.5765313837437418, 49.99999999999999289 ) ) ;
#3002 = CARTESIAN_POINT ( 'NONE',  ( -22.30770786884145451, 30.52886280891152282, 122.9933582338429972 ) ) ;
#3003 = AXIS2_PLACEMENT_3D ( 'NONE', #2133, #15339, #20298 ) ;
#3004 = DIRECTION ( 'NONE',  ( 0.000000000000000000, 0.000000000000000000, 1.000000000000000000 ) ) ;
#3005 = CARTESIAN_POINT ( 'NONE',  ( -45.43829269268869098, 234.1823905683720284, 3.332260488124734632 ) ) ;
#3006 = CARTESIAN_POINT ( 'NONE',  ( -22.27502019258946930, 308.4948905683720568, 15.47720386886985189 ) ) ;
#3007 = CARTESIAN_POINT ( 'NONE',  ( -36.33955658999051508, 445.3698905601785327, -18.47759065022572855 ) ) ;
#3008 = CARTESIAN_POINT ( 'NONE',  ( -28.68588794268871567, 379.7448905601785327, 19.99999999999999289 ) ) ;
#3009 = EDGE_CURVE ( 'NONE', #20997, #1814, #18022, .T. ) ;
#3010 = CARTESIAN_POINT ( 'NONE',  ( -14.48388495494899075, 299.4323905683720568, 9.489475012073732785 ) ) ;
#3011 = CARTESIAN_POINT ( 'NONE',  ( -42.88789093042843348, 354.8073905683720568, 9.489475012073736337 ) ) ;
#3012 = CARTESIAN_POINT ( 'NONE',  ( -28.68588794268873698, 522.8698905683719431, -16.75240474999999307 ) ) ;
#3013 = CARTESIAN_POINT ( 'NONE',  ( -8.685887942688722774, 371.9323905601784759, 3.978247347593161010 ) ) ;
#3014 = VECTOR ( 'NONE', #8793, 1000.000000000000000 ) ;
#3015 = PLANE ( 'NONE',  #6328 ) ;
#3016 = ORIENTED_EDGE ( 'NONE', *, *, #19278, .T. ) ;
#3017 = CARTESIAN_POINT ( 'NONE',  ( -25.35362745456399480, 488.1823905683720568, 16.75240474999998952 ) ) ;
#3018 = FILL_AREA_STYLE_COLOUR ( '', #80 ) ;
#3019 = CARTESIAN_POINT ( 'NONE',  ( -44.16309181155856578, 283.2448905683720568, -6.410867750099231266 ) ) ;
#3020 = ORIENTED_EDGE ( 'NONE', *, *, #8089, .F. ) ;
#3021 = EDGE_CURVE ( 'NONE', #258, #10312, #4626, .T. ) ;
#3022 = CARTESIAN_POINT ( 'NONE',  ( -14.48388495494898898, 289.4323905683720000, 9.489475012073731008 ) ) ;
#3023 = CARTESIAN_POINT ( 'NONE',  ( -40.53162694259543031, 315.1198905683720568, 11.84573899990672885 ) ) ;
#3024 = CARTESIAN_POINT ( 'NONE',  ( -44.16309181155855157, 265.9948905683720000, 6.410867750099241924 ) ) ;
#3025 = CIRCLE ( 'NONE', #1641, 50.00000000000000000 ) ;
#3026 = CARTESIAN_POINT ( 'NONE',  ( -10.20829729246297646, 267.6198905765655809, -7.653668647301794969 ) ) ;
#3027 = CARTESIAN_POINT ( 'NONE',  ( -28.68588794268874054, 573.2448905601785327, 0.000000000000000000 ) ) ;
#3028 = CARTESIAN_POINT ( 'NONE',  ( -44.16309181155855867, 233.2448905683720000, -6.410867750099231266 ) ) ;
#3029 = CARTESIAN_POINT ( 'NONE',  ( -32.01814843081344719, 377.5573905683720568, 16.75240474999999307 ) ) ;
#3030 = CARTESIAN_POINT ( 'NONE',  ( -43.52287249567941529, 200.6548609068916278, 2.226397062484288814 ) ) ;
#3031 = CARTESIAN_POINT ( 'NONE',  ( 5.074999999999999289, 3.752776749732560368, -6.499999999999999112 ) ) ;
#3032 = PRODUCT_DEFINITION_SHAPE ( 'NONE', 'NONE',  #15858 ) ;
#3033 = CARTESIAN_POINT ( 'NONE',  ( -45.64106924314017277, 271.0573905765656946, -11.32908994701042538 ) ) ;
#3034 = CARTESIAN_POINT ( 'NONE',  ( -32.01814843081345430, 416.0573905683720568, 16.75240474999999307 ) ) ;
#3035 = PLANE ( 'NONE',  #5313 ) ;
#3036 = VERTEX_POINT ( 'NONE', #19754 ) ;
#3037 = CARTESIAN_POINT ( 'NONE',  ( -21.03221929538691626, 430.3698905601784759, 18.47759065022572500 ) ) ;
#3038 = ORIENTED_EDGE ( 'NONE', *, *, #21080, .F. ) ;
#3039 = ORIENTED_EDGE ( 'NONE', *, *, #17623, .F. ) ;
#3040 = VERTEX_POINT ( 'NONE', #3322 ) ;
#3041 = DIRECTION ( 'NONE',  ( -1.191790137725560488E-16, 1.000000000000000000, 0.000000000000000000 ) ) ;
#3042 = CARTESIAN_POINT ( 'NONE',  ( -10.20829729246298001, 312.8698905601784759, -7.653668647301794969 ) ) ;
#3043 = FACE_OUTER_BOUND ( 'NONE', #5845, .T. ) ;
#3044 = CARTESIAN_POINT ( 'NONE',  ( -40.53162694259543741, 346.6198905683720000, 11.84573899990672885 ) ) ;
#3045 = CARTESIAN_POINT ( 'NONE',  ( -11.73070664223726389, 496.0573905765656377, 11.32908994701042005 ) ) ;
#3046 = CARTESIAN_POINT ( 'NONE',  ( -32.01814843081344719, 376.0573905683720000, 16.75240474999999307 ) ) ;
#3047 = CARTESIAN_POINT ( 'NONE',  ( -22.27502019258945865, 228.4948905683720284, 15.47720386886985189 ) ) ;
#3048 = CARTESIAN_POINT ( 'NONE',  ( -40.53162694259543741, 385.1198905683720568, 11.84573899990672885 ) ) ;
#3049 = CARTESIAN_POINT ( 'NONE',  ( -17.35679799567828852, 315.4323905765656377, 16.95518130045146421 ) ) ;
#3050 = FACE_OUTER_BOUND ( 'NONE', #2380, .T. ) ;
#3051 = CARTESIAN_POINT ( 'NONE',  ( -45.43829269268870519, 283.8698905683720568, 0.000000000000000000 ) ) ;
#3052 =( NAMED_UNIT ( * ) SI_UNIT ( $, .STERADIAN. ) SOLID_ANGLE_UNIT ( ) );
#3053 = CARTESIAN_POINT ( 'NONE',  ( -25.35362745456399125, 438.1823905683720000, 16.75240474999998952 ) ) ;
#3054 = CARTESIAN_POINT ( 'NONE',  ( -45.64106924314017277, 286.3073905601785327, -11.32908994701042538 ) ) ;
#3055 = LINE ( 'NONE', #14531, #2801 ) ;
#3056 = CARTESIAN_POINT ( 'NONE',  ( -8.685887942688742314, 573.2448905601785327, 2.449293598294706119E-15 ) ) ;
#3057 = CARTESIAN_POINT ( 'NONE',  ( -22.27502019258948707, 352.2448905683720000, -15.47720386886985544 ) ) ;
#3058 = CARTESIAN_POINT ( 'NONE',  ( -16.84014894278200813, 500.1198905683720000, -11.84573899990672707 ) ) ;
#3059 = CARTESIAN_POINT ( 'NONE',  ( -42.82802356641967378, 485.9948905601784759, -14.14213562373094746 ) ) ;
#3060 = CARTESIAN_POINT ( 'NONE',  ( -14.48388495494899431, 327.9323905683720568, 9.489475012073732785 ) ) ;
#3061 = VERTEX_POINT ( 'NONE', #9902 ) ;
#3062 = DIRECTION ( 'NONE',  ( 0.000000000000000000, -1.000000000000000000, 0.000000000000000000 ) ) ;
#3063 = ORIENTED_EDGE ( 'NONE', *, *, #20806, .T. ) ;
#3064 = CARTESIAN_POINT ( 'NONE',  ( 40.42502041961814996, 170.1716627696692683, -20.00000000000000355 ) ) ;
#3065 = ADVANCED_FACE ( 'NONE', ( #16524, #8276 ), #13386, .T. ) ;
#3066 = AXIS2_PLACEMENT_3D ( 'NONE', #16187, #11087, #4703 ) ;
#3067 = CARTESIAN_POINT ( 'NONE',  ( -11.93348319268872615, 410.6823905683720000, -3.332260488124732856 ) ) ;
#3068 = CARTESIAN_POINT ( 'NONE',  ( -28.68588794268869790, 234.4948905765656377, 19.99999999999999289 ) ) ;
#3069 = CARTESIAN_POINT ( 'NONE',  ( -48.68588794268873698, 573.2448905601785327, 0.000000000000000000 ) ) ;
#3070 = CARTESIAN_POINT ( 'NONE',  ( -11.93348319268873148, 448.5573905683720000, 3.332260488124728415 ) ) ;
#3071 = CARTESIAN_POINT ( 'NONE',  ( -13.20868407381887089, 449.4948905683720568, -6.410867750099233042 ) ) ;
#3072 = DIRECTION ( 'NONE',  ( 0.000000000000000000, 0.000000000000000000, 1.000000000000000000 ) ) ;
#3073 = CARTESIAN_POINT ( 'NONE',  ( -17.35679799567830273, 413.8073905601785327, -16.95518130045146421 ) ) ;
#3074 = CARTESIAN_POINT ( 'NONE',  ( -24.70764059509555466, 384.8073905765655809, 19.99999999999998934 ) ) ;
#3075 = DIRECTION ( 'NONE',  ( -1.000000000000000000, 0.000000000000000000, 0.000000000000000000 ) ) ;
#3076 = CARTESIAN_POINT ( 'NONE',  ( -48.68588794268855224, 391.6823905765656377, -3.978247347593583783 ) ) ;
#3077 = CARTESIAN_POINT ( 'NONE',  ( 44.98449999999999704, 4.898587196589412829E-16, -4.000000000000000000 ) ) ;
#3078 = DIRECTION ( 'NONE',  ( 0.000000000000000000, 0.000000000000000000, -1.000000000000000000 ) ) ;
#3079 = CARTESIAN_POINT ( 'NONE',  ( -32.01814843081346140, 497.5573905683720568, 16.75240474999999307 ) ) ;
#3080 = CARTESIAN_POINT ( 'NONE',  ( 71.32175588950862277, 75.31183677523708297, -94.99999999999994316 ) ) ;
#3081 = DIRECTION ( 'NONE',  ( 0.000000000000000000, 0.000000000000000000, 1.000000000000000000 ) ) ;
#3082 = CARTESIAN_POINT ( 'NONE',  ( -45.21523660720509952, 223.9102039777117454, 6.319766016702155653 ) ) ;
#3083 = AXIS2_PLACEMENT_3D ( 'NONE', #379, #13571, #5328 ) ;
#3084 = ADVANCED_FACE ( 'NONE', ( #13280 ), #3533, .T. ) ;
#3085 = CARTESIAN_POINT ( 'NONE',  ( -38.17536295476245556, 406.9323905683719431, 14.20200298773971781 ) ) ;
#3086 = DIRECTION ( 'NONE',  ( -1.000000000000000000, 0.000000000000000000, 0.000000000000000000 ) ) ;
#3087 = CARTESIAN_POINT ( 'NONE',  ( -35.09675569278793006, 223.4948905683720284, -15.47720386886985544 ) ) ;
#3088 = ORIENTED_EDGE ( 'NONE', *, *, #18213, .T. ) ;
#3089 = EDGE_LOOP ( 'NONE', ( #16242, #14565, #17246, #12295 ) ) ;
#3090 = DIRECTION ( 'NONE',  ( 0.000000000000000000, 0.000000000000000000, 1.000000000000000000 ) ) ;
#3091 = EDGE_LOOP ( 'NONE', ( #12081, #398, #11971, #422 ) ) ;
#3092 = CIRCLE ( 'NONE', #14161, 125.0000000000000000 ) ;
#3093 = CARTESIAN_POINT ( 'NONE',  ( -35.09675569278795848, 463.4948905683720000, -15.47720386886985544 ) ) ;
#3094 = CARTESIAN_POINT ( 'NONE',  ( -10.20829729246297113, 227.6198905765656093, -7.653668647301794969 ) ) ;
#3095 = EDGE_LOOP ( 'NONE', ( #18663, #20973, #2382, #1209 ) ) ;
#3096 = CARTESIAN_POINT ( 'NONE',  ( -43.68588794268870856, 210.1437886375728965, 0.3278592396120688091 ) ) ;
#3097 = CARTESIAN_POINT ( 'NONE',  ( -19.19641293061500420, 531.9323905683720568, -14.20200298773971603 ) ) ;
#3098 = EDGE_LOOP ( 'NONE', ( #21304, #3311, #17459 ) ) ;
#3099 = CARTESIAN_POINT ( 'NONE',  ( -40.53162694259545873, 515.1198905683720568, 11.84573899990672885 ) ) ;
#3100 = DIRECTION ( 'NONE',  ( -0.000000000000000000, -0.000000000000000000, 1.000000000000000000 ) ) ;
#3101 = VECTOR ( 'NONE', #20232, 999.9999999999998863 ) ;
#3102 = EDGE_CURVE ( 'NONE', #19703, #13742, #19865, .T. ) ;
#3103 = CARTESIAN_POINT ( 'NONE',  ( -47.16347859291445133, 441.3698905765656377, -7.653668647301793193 ) ) ;
#3104 = CARTESIAN_POINT ( 'NONE',  ( -28.68588794268869435, 188.9102039777116602, 0.000000000000000000 ) ) ;
#3105 = CARTESIAN_POINT ( 'NONE',  ( -11.93348319268871904, 338.8698905683720000, -2.051577885510841163E-15 ) ) ;
#3106 = CARTESIAN_POINT ( 'NONE',  ( -14.54375231895777887, 455.7448905765656377, 14.14213562373094568 ) ) ;
#3107 = DIRECTION ( 'NONE',  ( 0.000000000000000000, -1.000000000000000000, 9.855701800883825964E-17 ) ) ;
#3108 = DIRECTION ( 'NONE',  ( 0.000000000000000000, -1.000000000000000000, 0.000000000000000000 ) ) ;
#3109 = VECTOR ( 'NONE', #6523, 1000.000000000000000 ) ;
#3110 = DIRECTION ( 'NONE',  ( 0.000000000000000000, -0.000000000000000000, 1.000000000000000000 ) ) ;
#3111 = CARTESIAN_POINT ( 'NONE',  ( 2.416697501590669095, 217.7548513357008630, 49.99999999999999289 ) ) ;
#3112 = CARTESIAN_POINT ( 'NONE',  ( -44.16309181155855867, 325.9948905683720000, 6.410867750099241924 ) ) ;
#3113 = EDGE_CURVE ( 'NONE', #11304, #17379, #18237, .T. ) ;
#3114 = CARTESIAN_POINT ( 'NONE',  ( 43.53705524234220547, -133.1434774248255906, -96.62835994548002816 ) ) ;
#3115 = CARTESIAN_POINT ( 'NONE',  ( -17.35679799567828141, 270.6823905601785327, 16.95518130045146421 ) ) ;
#3116 = FACE_OUTER_BOUND ( 'NONE', #21153, .T. ) ;
#3117 = CARTESIAN_POINT ( 'NONE',  ( -40.53162694259543031, 306.6198905683720000, 11.84573899990672885 ) ) ;
#3118 = CARTESIAN_POINT ( 'NONE',  ( -40.53162694259545873, 514.1198905683720568, -11.84573899990672707 ) ) ;
#3119 = CARTESIAN_POINT ( 'NONE',  ( -28.68588794268871212, 369.7448905601785327, 19.99999999999999289 ) ) ;
#3120 = CARTESIAN_POINT ( 'NONE',  ( -36.33955658999050087, 315.3698905601784759, -18.47759065022572855 ) ) ;
#3121 = ORIENTED_EDGE ( 'NONE', *, *, #16587, .F. ) ;
#3122 = CARTESIAN_POINT ( 'NONE',  ( -42.88789093042844769, 486.3073905683721136, 9.489475012073736337 ) ) ;
#3123 = CARTESIAN_POINT ( 'NONE',  ( -6.276925316985662029, 585.7448905601785327, 44.69718552705352010 ) ) ;
#3124 = CARTESIAN_POINT ( 'NONE',  ( -13.20868407381884779, 278.2448905683720568, 6.410867750099229490 ) ) ;
#3125 = VERTEX_POINT ( 'NONE', #1821 ) ;
#3126 = CARTESIAN_POINT ( 'NONE',  ( -16.84014894278198327, 291.6198905683720000, -11.84573899990672707 ) ) ;
#3127 = CARTESIAN_POINT ( 'NONE',  ( -13.20868407381885490, 319.4948905683720000, -6.410867750099233042 ) ) ;
#3128 = CARTESIAN_POINT ( 'NONE',  ( -8.685887942688710339, 256.9948905765655809, -2.449293598294705724E-15 ) ) ;
#3129 = AXIS2_PLACEMENT_3D ( 'NONE', #2154, #2581, #8735 ) ;
#3130 = CARTESIAN_POINT ( 'NONE',  ( 105.7989814974898479, 152.5259582928263740, 20.00000000000000355 ) ) ;
#3131 = CARTESIAN_POINT ( 'NONE',  ( -40.53162694259542320, 235.1198905683720000, 11.84573899990672885 ) ) ;
#3132 = CARTESIAN_POINT ( 'NONE',  ( -16.84014894278198682, 369.1198905683720000, 11.84573899990672530 ) ) ;
#3133 = CARTESIAN_POINT ( 'NONE',  ( -13.68588794268873521, 548.2448905601784190, 0.000000000000000000 ) ) ;
#3134 = AXIS2_PLACEMENT_3D ( 'NONE', #7876, #7454, #20884 ) ;
#3135 = AXIS2_PLACEMENT_3D ( 'NONE', #14923, #15926, #7687 ) ;
#3136 = EDGE_CURVE ( 'NONE', #4779, #469, #14736, .T. ) ;
#3137 = DIRECTION ( 'NONE',  ( -1.157565925312684532E-16, 0.9253149302858357794, -0.3791995250394160633 ) ) ;
#3138 = EDGE_CURVE ( 'NONE', #9575, #16161, #4914, .T. ) ;
#3139 = CARTESIAN_POINT ( 'NONE',  ( -32.01814843081345430, 431.6823905683720000, -16.75240474999999307 ) ) ;
#3140 = CARTESIAN_POINT ( 'NONE',  ( 79.78925230247502043, 142.5259582928263455, -20.00000000000000355 ) ) ;
#3141 = ORIENTED_EDGE ( 'NONE', *, *, #6501, .T. ) ;
#3142 = CARTESIAN_POINT ( 'NONE',  ( -47.16347859291445133, 427.8698905601784759, 7.653668647301805628 ) ) ;
#3143 = ORIENTED_EDGE ( 'NONE', *, *, #19941, .T. ) ;
#3144 = AXIS2_PLACEMENT_3D ( 'NONE', #12812, #11281, #19403 ) ;
#3145 = ORIENTED_EDGE ( 'NONE', *, *, #6536, .T. ) ;
#3146 = ORIENTED_EDGE ( 'NONE', *, *, #7946, .T. ) ;
#3147 = CARTESIAN_POINT ( 'NONE',  ( -48.68588794268870856, 351.9948905765656377, 0.000000000000000000 ) ) ;
#3148 = CARTESIAN_POINT ( 'NONE',  ( -14.54375231895776288, 303.4948905601784759, -14.14213562373094746 ) ) ;
#3149 = DIRECTION ( 'NONE',  ( 1.191790137725560488E-16, -1.000000000000000000, -0.000000000000000000 ) ) ;
#3150 = EDGE_CURVE ( 'NONE', #16453, #6197, #1668, .T. ) ;
#3151 = CARTESIAN_POINT ( 'NONE',  ( -35.09675569278795138, 337.2448905683720568, 15.47720386886985366 ) ) ;
#3152 = VECTOR ( 'NONE', #5219, 1000.000000000000000 ) ;
#3153 = AXIS2_PLACEMENT_3D ( 'NONE', #12038, #14005, #8684 ) ;
#3154 = CARTESIAN_POINT ( 'NONE',  ( -28.68588794268872988, 504.4948905765655809, 19.99999999999999289 ) ) ;
#3155 = CARTESIAN_POINT ( 'NONE',  ( -38.17536295476244845, 385.4323905683720000, 14.20200298773971781 ) ) ;
#3156 = CARTESIAN_POINT ( 'NONE',  ( -35.09675569278793716, 227.2448905683720568, 15.47720386886985366 ) ) ;
#3157 = CARTESIAN_POINT ( 'NONE',  ( -14.48388495494900674, 389.8073905683721136, -9.489475012073734561 ) ) ;
#3158 = ADVANCED_FACE ( 'NONE', ( #21127 ), #8125, .F. ) ;
#3159 = CARTESIAN_POINT ( 'NONE',  ( -40.01497788969913927, 330.4323905765655809, -16.95518130045146421 ) ) ;
#3160 = CARTESIAN_POINT ( 'NONE',  ( -45.64106924314018698, 426.3073905601784190, -11.32908994701042538 ) ) ;
#3161 = CARTESIAN_POINT ( 'NONE',  ( -25.35362745456398414, 291.0573905683720568, -16.75240474999999307 ) ) ;
#3162 = CARTESIAN_POINT ( 'NONE',  ( 0.000000000000000000, -343.0245277843623057, 0.000000000000000000 ) ) ;
#3163 = CARTESIAN_POINT ( 'NONE',  ( -22.27502019258948707, 438.4948905683720568, 15.47720386886985189 ) ) ;
#3164 = LINE ( 'NONE', #19916, #8179 ) ;
#3165 = CARTESIAN_POINT ( 'NONE',  ( -48.68588794268870856, 357.2448905601784759, 0.000000000000000000 ) ) ;
#3166 = CARTESIAN_POINT ( 'NONE',  ( 5.674999999999999822, 0.000000000000000000, 6.500000000000000888 ) ) ;
#3167 = DIRECTION ( 'NONE',  ( 0.000000000000000000, -0.5000000000000018874, -0.8660254037844374864 ) ) ;
#3168 = EDGE_CURVE ( 'NONE', #21019, #6223, #9543, .T. ) ;
#3169 = CARTESIAN_POINT ( 'NONE',  ( -11.93348319268872260, 340.6823905683720000, -3.332260488124732856 ) ) ;
#3170 = CARTESIAN_POINT ( 'NONE',  ( -40.53162694259545162, 492.6198905683720000, -11.84573899990672707 ) ) ;
#3171 = ORIENTED_EDGE ( 'NONE', *, *, #20988, .T. ) ;
#3172 = CARTESIAN_POINT ( 'NONE',  ( -28.68588794268872633, 479.7448905601784759, 19.99999999999999289 ) ) ;
#3173 = CARTESIAN_POINT ( 'NONE',  ( -13.20868407381885312, 299.4948905683720568, -6.410867750099233042 ) ) ;
#3174 = EDGE_LOOP ( 'NONE', ( #10900, #12243, #10849, #7499, #1832, #2487 ) ) ;
#3175 = DIRECTION ( 'NONE',  ( 1.000000000000000000, 0.000000000000000000, -0.000000000000000000 ) ) ;
#3176 = EDGE_LOOP ( 'NONE', ( #13530, #14546, #13118, #14686 ) ) ;
#3177 = CARTESIAN_POINT ( 'NONE',  ( 60.03793209889851568, 30.52886280891152282, -131.1729372809869005 ) ) ;
#3178 = CARTESIAN_POINT ( 'NONE',  ( -14.48388495494900674, 411.3073905683720000, -9.489475012073734561 ) ) ;
#3179 = DIRECTION ( 'NONE',  ( 0.000000000000000000, 0.000000000000000000, 1.000000000000000000 ) ) ;
#3180 = CARTESIAN_POINT ( 'NONE',  ( 18.20947592957839234, 600.7448905601785327, 168.5995991907681457 ) ) ;
#3181 = CARTESIAN_POINT ( 'NONE',  ( -28.68588794268872633, 451.3698905683720000, -16.75240474999999307 ) ) ;
#3182 = CARTESIAN_POINT ( 'NONE',  ( -42.88789093042844058, 442.9323905683720568, -9.489475012073734561 ) ) ;
#3183 = LINE ( 'NONE', #14661, #16919 ) ;
#3184 = CARTESIAN_POINT ( 'NONE',  ( -17.35679799567830273, 378.5573905765656946, -16.95518130045146421 ) ) ;
#3185 = CARTESIAN_POINT ( 'NONE',  ( -48.68588794268870856, 361.9948905765655809, 0.000000000000000000 ) ) ;
#3186 = DIRECTION ( 'NONE',  ( -1.000000000000000000, 0.000000000000000000, 0.000000000000000000 ) ) ;
#3187 = LINE ( 'NONE', #19617, #16718 ) ;
#3188 = CARTESIAN_POINT ( 'NONE',  ( -32.66413529028185536, 254.1823905765656377, 19.99999999999999289 ) ) ;
#3189 = COLOUR_RGB ( '',0.7921568627450980005, 0.8196078431372548767, 0.9333333333333333481 ) ;
#3190 = CARTESIAN_POINT ( 'NONE',  ( -45.43829269268872650, 495.3698905683720568, 0.000000000000000000 ) ) ;
#3191 = CARTESIAN_POINT ( 'NONE',  ( 45.67500000000000426, 0.000000000000000000, 0.000000000000000000 ) ) ;
#3192 = CARTESIAN_POINT ( 'NONE',  ( -54.57497958038185004, 230.5765313837437418, 49.99999999999999289 ) ) ;
#3193 = ADVANCED_FACE ( 'NONE', ( #11272 ), #9857, .T. ) ;
#3194 = CARTESIAN_POINT ( 'NONE',  ( -43.04742826731176564, 207.6584868706943041, 4.333760535973598671 ) ) ;
#3195 = CARTESIAN_POINT ( 'NONE',  ( -44.16309181155857289, 415.9948905683720000, 6.410867750099241924 ) ) ;
#3196 = CARTESIAN_POINT ( 'NONE',  ( -36.33955658999052218, 470.1198905765656377, -18.47759065022572855 ) ) ;
#3197 = CARTESIAN_POINT ( 'NONE',  ( -32.01814843081343298, 233.1823905683720284, -16.75240474999999307 ) ) ;
#3198 = EDGE_LOOP ( 'NONE', ( #21307, #15771, #9946, #212 ) ) ;
#3199 = PLANE ( 'NONE',  #17563 ) ;
#3200 = ORIENTED_EDGE ( 'NONE', *, *, #20326, .T. ) ;
#3201 = CARTESIAN_POINT ( 'NONE',  ( -38.17536295476246977, 453.8073905683720568, -14.20200298773971426 ) ) ;
#3202 = VECTOR ( 'NONE', #7993, 1000.000000000000000 ) ;
#3203 = CARTESIAN_POINT ( 'NONE',  ( -8.685887942688706786, 227.3073905765656093, -3.978247347593165895 ) ) ;
#3204 = EDGE_LOOP ( 'NONE', ( #5315, #16301, #13071, #14291, #3360 ) ) ;
#3205 = DIRECTION ( 'NONE',  ( -0.000000000000000000, -0.000000000000000000, -1.000000000000000000 ) ) ;
#3206 = CARTESIAN_POINT ( 'NONE',  ( -38.17536295476246977, 526.9323905683719431, 14.20200298773971781 ) ) ;
#3207 = ORIENTED_EDGE ( 'NONE', *, *, #20195, .F. ) ;
#3208 = CARTESIAN_POINT ( 'NONE',  ( -14.48388495494901385, 507.9323905683720000, 9.489475012073731008 ) ) ;
#3209 = CARTESIAN_POINT ( 'NONE',  ( 35.96497763894178945, 170.1716627696692683, 20.00000000000000355 ) ) ;
#3210 = EDGE_CURVE ( 'NONE', #12803, #16558, #16162, .T. ) ;
#3211 = CARTESIAN_POINT ( 'NONE',  ( -48.68588794268872277, 451.9948905765656377, 0.000000000000000000 ) ) ;
#3212 = CARTESIAN_POINT ( 'NONE',  ( -24.70764059509555111, 299.1823905765656377, -19.99999999999999289 ) ) ;
#3213 = LINE ( 'NONE', #14796, #5776 ) ;
#3214 = CARTESIAN_POINT ( 'NONE',  ( -48.68588794268869435, 247.2448905601785043, 0.000000000000000000 ) ) ;
#3215 = LINE ( 'NONE', #6231, #461 ) ;
#3216 = CARTESIAN_POINT ( 'NONE',  ( -28.68588794268874409, 608.2448905601786464, -20.00000000000000000 ) ) ;
#3217 = VECTOR ( 'NONE', #4795, 1000.000000000000000 ) ;
#3218 = CARTESIAN_POINT ( 'NONE',  ( 162.8695233526006803, 620.7448905601785327, -10.81142786866620575 ) ) ;
#3219 = FACE_OUTER_BOUND ( 'NONE', #15290, .T. ) ;
#3220 = CARTESIAN_POINT ( 'NONE',  ( -11.93348319268871727, 320.6823905683720000, -3.332260488124732856 ) ) ;
#3221 = DIRECTION ( 'NONE',  ( -0.000000000000000000, -0.000000000000000000, 1.000000000000000000 ) ) ;
#3222 = CARTESIAN_POINT ( 'NONE',  ( -14.54375231895775933, 273.4948905601785327, -14.14213562373094746 ) ) ;
#3223 = DIRECTION ( 'NONE',  ( 0.000000000000000000, 1.000000000000000000, -0.000000000000000000 ) ) ;
#3224 = CARTESIAN_POINT ( 'NONE',  ( -44.16309181155855867, 295.9948905683720000, 6.410867750099241924 ) ) ;
#3225 = EDGE_CURVE ( 'NONE', #14751, #13685, #1339, .T. ) ;
#3226 = VECTOR ( 'NONE', #10704, 1000.000000000000000 ) ;
#3227 = CARTESIAN_POINT ( 'NONE',  ( -11.93348319268874214, 530.0573905683720568, 3.332260488124728859 ) ) ;
#3228 = AXIS2_PLACEMENT_3D ( 'NONE', #13866, #15600, #2824 ) ;
#3229 = CARTESIAN_POINT ( 'NONE',  ( -47.16347859291444422, 357.8698905601784759, 7.653668647301805628 ) ) ;
#3230 = CARTESIAN_POINT ( 'NONE',  ( -11.73070664223723369, 227.9323905765656377, -11.32908994701042538 ) ) ;
#3231 = ORIENTED_EDGE ( 'NONE', *, *, #17240, .F. ) ;
#3232 = CARTESIAN_POINT ( 'NONE',  ( -45.43829269268871940, 485.6823905683721136, 3.332260488124734632 ) ) ;
#3233 = CARTESIAN_POINT ( 'NONE',  ( -25.35362745456398059, 281.0573905683720568, -16.75240474999999307 ) ) ;
#3234 = ORIENTED_EDGE ( 'NONE', *, *, #8416, .F. ) ;
#3235 = EDGE_CURVE ( 'NONE', #6356, #19050, #1779, .T. ) ;
#3236 = CARTESIAN_POINT ( 'NONE',  ( -28.68588794268870146, 277.8698905683720000, 16.75240474999999307 ) ) ;
#3237 = CARTESIAN_POINT ( 'NONE',  ( -45.43829269268869808, 255.6823905683720000, 3.332260488124734632 ) ) ;
#3238 = VECTOR ( 'NONE', #10633, 1000.000000000000000 ) ;
#3239 = CARTESIAN_POINT ( 'NONE',  ( -8.685887942688708563, 246.9948905765656093, -2.449293598294705724E-15 ) ) ;
#3240 = DIRECTION ( 'NONE',  ( -1.000000000000000000, 0.000000000000000000, 0.000000000000000000 ) ) ;
#3241 = CARTESIAN_POINT ( 'NONE',  ( -44.16309181155855157, 234.4948905683720284, 6.410867750099241924 ) ) ;
#3242 = CIRCLE ( 'NONE', #14646, 10.00000000000000178 ) ;
#3243 = CARTESIAN_POINT ( 'NONE',  ( -45.43829269268870519, 375.0573905683720000, -3.332260488124726194 ) ) ;
#3244 = CARTESIAN_POINT ( 'NONE',  ( -14.54375231895775578, 280.9948905601785327, 14.14213562373094568 ) ) ;
#3245 = CARTESIAN_POINT ( 'NONE',  ( -45.64106924314019409, 461.0573905765656377, -11.32908994701042538 ) ) ;
#3246 = DIRECTION ( 'NONE',  ( -0.9864615503757148129, 0.000000000000000000, 0.1639927121256942455 ) ) ;
#3247 = CARTESIAN_POINT ( 'NONE',  ( -14.48388495494900496, 427.9323905683720568, 9.489475012073732785 ) ) ;
#3248 = DIRECTION ( 'NONE',  ( 1.000000000000000000, 0.000000000000000000, 0.000000000000000000 ) ) ;
#3249 = ORIENTED_EDGE ( 'NONE', *, *, #10862, .T. ) ;
#3250 = CARTESIAN_POINT ( 'NONE',  ( -14.54375231895777887, 433.4948905601784759, -14.14213562373094746 ) ) ;
#3251 = EDGE_LOOP ( 'NONE', ( #19896, #13797, #2612, #9442 ) ) ;
#3252 = DIRECTION ( 'NONE',  ( 0.000000000000000000, 0.000000000000000000, -1.000000000000000000 ) ) ;
#3253 = ORIENTED_EDGE ( 'NONE', *, *, #18866, .T. ) ;
#3254 = ORIENTED_EDGE ( 'NONE', *, *, #6927, .T. ) ;
#3255 = CARTESIAN_POINT ( 'NONE',  ( -43.31915179403467420, 208.9097650327693430, -3.305147470758842410 ) ) ;
#3256 = CARTESIAN_POINT ( 'NONE',  ( -10.20829729246297823, 311.6198905601784759, 7.653668647301790529 ) ) ;
#3257 = CARTESIAN_POINT ( 'NONE',  ( -28.68588794268872633, 378.8848358243226357, 0.000000000000000000 ) ) ;
#3258 = AXIS2_PLACEMENT_3D ( 'NONE', #17874, #19606, #19932 ) ;
#3259 = CARTESIAN_POINT ( 'NONE',  ( -45.43829269268871229, 345.6823905683720000, 3.332260488124734632 ) ) ;
#3260 = CARTESIAN_POINT ( 'NONE',  ( -24.70764059509556532, 474.8073905765655809, 19.99999999999998934 ) ) ;
#3261 = CARTESIAN_POINT ( 'NONE',  ( -13.20868407381885845, 358.2448905683720000, 6.410867750099229490 ) ) ;
#3262 = CARTESIAN_POINT ( 'NONE',  ( -14.48388495494898187, 229.4323905683720000, 9.489475012073732785 ) ) ;
#3263 = CARTESIAN_POINT ( 'NONE',  ( -45.43829269268871940, 393.8698905683720000, 0.000000000000000000 ) ) ;
#3264 =( BOUNDED_CURVE ( )  B_SPLINE_CURVE ( 2, ( #17062, #5580, #20405, #627, #4170, #13928, #5685, #13708, #7516, #15341, #15761, #5900, #7192, #7086, #2558, #3852, #14140 ),
 .UNSPECIFIED., .F., .T. ) 
 B_SPLINE_CURVE_WITH_KNOTS ( ( 3, 2, 2, 2, 2, 2, 2, 2, 3 ),
 ( 0.4062500000000001665, 0.4082031250000001665, 0.4101562500000001665, 0.4121093750000001665, 0.4140625000000001665, 0.4160156250000001665, 0.4179687500000001665, 0.4199218750000001665, 0.4218750000000001665 ),
 .UNSPECIFIED. ) 
 CURVE ( )  GEOMETRIC_REPRESENTATION_ITEM ( )  RATIONAL_B_SPLINE_CURVE ( ( 0.9999999999999983347, 0.9807852804032320959, 1.000000000000000000, 0.9807852804032304306, 1.000000000000000000, 0.9807852804032304306, 1.000000000000000000, 0.9807852804032304306, 1.000000000000000000, 0.9807852804032304306, 1.000000000000000000, 0.9807852804032304306, 1.000000000000000000, 0.9807852804032304306, 1.000000000000000000, 0.9807852804032287652, 1.000000000000001554 ) ) 
 REPRESENTATION_ITEM ( '' )  );
#3265 = CARTESIAN_POINT ( 'NONE',  ( -32.66413529028186957, 314.1823905765655809, 19.99999999999999289 ) ) ;
#3266 = DIRECTION ( 'NONE',  ( -1.000000000000000000, 0.000000000000000000, 2.775557561562891844E-16 ) ) ;
#3267 = CARTESIAN_POINT ( 'NONE',  ( -38.17536295476244845, 292.3073905683720000, -14.20200298773971426 ) ) ;
#3268 = CARTESIAN_POINT ( 'NONE',  ( -18.68588794268873698, 281.1055109169419666, -20.00000000000000355 ) ) ;
#3269 = CARTESIAN_POINT ( 'NONE',  ( -11.93348319268872970, 430.0573905683721136, 3.332260488124728415 ) ) ;
#3270 = CARTESIAN_POINT ( 'NONE',  ( -33.84809828339280102, 56.85652257517428865, 120.3299889578561448 ) ) ;
#3271 = DIRECTION ( 'NONE',  ( -1.000000000000000000, -0.000000000000000000, -0.000000000000000000 ) ) ;
#3272 = FACE_OUTER_BOUND ( 'NONE', #9149, .T. ) ;
#3273 = CARTESIAN_POINT ( 'NONE',  ( -45.43829269268873361, 533.8698905683720568, 0.000000000000000000 ) ) ;
#3274 = EDGE_CURVE ( 'NONE', #3284, #15800, #1902, .T. ) ;
#3275 = CARTESIAN_POINT ( 'NONE',  ( -22.27502019258947286, 338.4948905683720568, 15.47720386886985189 ) ) ;
#3276 = CARTESIAN_POINT ( 'NONE',  ( -32.01814843081346140, 481.6823905683720568, -16.75240474999999307 ) ) ;
#3277 = ADVANCED_FACE ( 'NONE', ( #4782 ), #8237, .T. ) ;
#3278 = ORIENTED_EDGE ( 'NONE', *, *, #13849, .F. ) ;
#3279 = CARTESIAN_POINT ( 'NONE',  ( -24.70764059509557953, 494.4323905601783622, -19.99999999999999289 ) ) ;
#3280 = CARTESIAN_POINT ( 'NONE',  ( -45.43829269268870519, 303.8698905683720000, 0.000000000000000000 ) ) ;
#3281 = EDGE_CURVE ( 'NONE', #11550, #19077, #6400, .T. ) ;
#3282 = EDGE_LOOP ( 'NONE', ( #21260, #654, #1914, #18858 ) ) ;
#3283 = CARTESIAN_POINT ( 'NONE',  ( 60.03793209889851568, 10.52886280891152104, 126.1729372809868863 ) ) ;
#3284 = VERTEX_POINT ( 'NONE', #4895 ) ;
#3285 = CARTESIAN_POINT ( 'NONE',  ( 166.1493775951145437, 610.7448905601785327, 8.917803138848105604 ) ) ;
#3286 = CARTESIAN_POINT ( 'NONE',  ( -13.20868407381886378, 399.7448905683720568, 6.410867750099229490 ) ) ;
#3287 = CARTESIAN_POINT ( 'NONE',  ( 60.03793209889851568, 30.52886280891152282, -152.3753892284480003 ) ) ;
#3288 = FACE_OUTER_BOUND ( 'NONE', #18886, .T. ) ;
#3289 = CARTESIAN_POINT ( 'NONE',  ( -25.35362745456399836, 431.0573905683720000, -16.75240474999999307 ) ) ;
#3290 = CARTESIAN_POINT ( 'NONE',  ( -25.35362745456399125, 446.6823905683720568, 16.75240474999998952 ) ) ;
#3291 = DIRECTION ( 'NONE',  ( 0.000000000000000000, 0.000000000000000000, 1.000000000000000000 ) ) ;
#3292 = FACE_OUTER_BOUND ( 'NONE', #877, .T. ) ;
#3293 = ADVANCED_FACE ( 'NONE', ( #5003 ), #44, .T. ) ;
#3294 = CARTESIAN_POINT ( 'NONE',  ( -8.685887942688724550, 386.6823905765655809, 3.978247347593161010 ) ) ;
#3295 = FACE_OUTER_BOUND ( 'NONE', #10572, .T. ) ;
#3296 = CARTESIAN_POINT ( 'NONE',  ( 78.68120802659203150, 149.7457237375499517, 94.99999999999994316 ) ) ;
#3297 = DIRECTION ( 'NONE',  ( 0.8865057725575725689, 0.000000000000000000, 0.4627175328665443232 ) ) ;
#3298 = DIRECTION ( 'NONE',  ( 0.000000000000000000, 0.000000000000000000, -1.000000000000000000 ) ) ;
#3299 = CARTESIAN_POINT ( 'NONE',  ( -25.35362745456400901, 492.5573905683721136, -16.75240474999999307 ) ) ;
#3300 = CARTESIAN_POINT ( 'NONE',  ( -8.685887942688717445, 312.2448905601784759, -2.449293598294705724E-15 ) ) ;
#3301 = CARTESIAN_POINT ( 'NONE',  ( -8.685887942688733432, 462.2448905601784759, -2.449293598294705724E-15 ) ) ;
#3302 = CARTESIAN_POINT ( 'NONE',  ( -28.68588794268872633, 378.8848358243226357, 0.000000000000000000 ) ) ;
#3303 = CARTESIAN_POINT ( 'NONE',  ( -16.84014894278199392, 401.6198905683720568, -11.84573899990672707 ) ) ;
#3304 = LINE ( 'NONE', #14993, #13713 ) ;
#3305 = CARTESIAN_POINT ( 'NONE',  ( -45.43829269268869098, 225.0573905683720568, -3.332260488124726194 ) ) ;
#3306 = ORIENTED_EDGE ( 'NONE', *, *, #9439, .F. ) ;
#3307 = DIRECTION ( 'NONE',  ( -1.000000000000000000, 0.000000000000000000, 0.000000000000000000 ) ) ;
#3308 = ORIENTED_EDGE ( 'NONE', *, *, #21108, .F. ) ;
#3309 = CARTESIAN_POINT ( 'NONE',  ( -44.16309181155857289, 435.9948905683720568, 6.410867750099241924 ) ) ;
#3310 = CARTESIAN_POINT ( 'NONE',  ( -40.53162694259545873, 525.1198905683720568, 11.84573899990672885 ) ) ;
#3311 = ORIENTED_EDGE ( 'NONE', *, *, #4592, .F. ) ;
#3312 = LINE ( 'NONE', #11093, #13160 ) ;
#3313 = CARTESIAN_POINT ( 'NONE',  ( -28.68588794268869435, 226.3698905683720284, 16.75240474999999307 ) ) ;
#3314 = ORIENTED_EDGE ( 'NONE', *, *, #18512, .T. ) ;
#3315 = CARTESIAN_POINT ( 'NONE',  ( -11.93348319268873858, 508.5573905683720000, 3.332260488124728859 ) ) ;
#3316 = DIRECTION ( 'NONE',  ( 0.000000000000000000, -1.000000000000000000, 0.000000000000000000 ) ) ;
#3317 = CARTESIAN_POINT ( 'NONE',  ( -14.54375231895777532, 435.7448905765656377, 14.14213562373094568 ) ) ;
#3318 = CARTESIAN_POINT ( 'NONE',  ( -11.73070664223724968, 357.9323905765656377, -11.32908994701042538 ) ) ;
#3319 = CARTESIAN_POINT ( 'NONE',  ( -8.685887942688895080, 331.9323905601783622, 3.978247347593586447 ) ) ;
#3320 = CARTESIAN_POINT ( 'NONE',  ( 81.24038404635965094, 10.52886280891152104, 131.1729372809869005 ) ) ;
#3321 = DIRECTION ( 'NONE',  ( 0.000000000000000000, -0.000000000000000000, -1.000000000000000000 ) ) ;
#3322 = CARTESIAN_POINT ( 'NONE',  ( -8.685887942688708563, 246.9948905765656093, -2.449293598294705724E-15 ) ) ;
#3323 = DIRECTION ( 'NONE',  ( 0.000000000000000000, 0.000000000000000000, -1.000000000000000000 ) ) ;
#3324 = CARTESIAN_POINT ( 'NONE',  ( -14.48388495494898898, 289.4323905683720000, 9.489475012073732785 ) ) ;
#3325 = DIRECTION ( 'NONE',  ( 1.000000000000000000, 0.000000000000000000, 0.000000000000000000 ) ) ;
#3326 = CARTESIAN_POINT ( 'NONE',  ( -47.16347859291443712, 276.6198905601784759, -7.653668647301793193 ) ) ;
#3327 = CARTESIAN_POINT ( 'NONE',  ( -18.66797547166049753, 223.9102039777116602, -17.31025331282116397 ) ) ;
#3328 = CARTESIAN_POINT ( 'NONE',  ( -35.09675569278794427, 297.2448905683720000, 15.47720386886985366 ) ) ;
#3329 = EDGE_CURVE ( 'NONE', #19472, #18782, #19828, .T. ) ;
#3330 = CARTESIAN_POINT ( 'NONE',  ( -40.53162694259545162, 504.1198905683720568, -11.84573899990672707 ) ) ;
#3331 = CARTESIAN_POINT ( 'NONE',  ( -42.82802356641965957, 368.4948905601784759, 14.14213562373094923 ) ) ;
#3332 = VECTOR ( 'NONE', #8114, 1000.000000000000000 ) ;
#3333 = CARTESIAN_POINT ( 'NONE',  ( -32.66413529028186247, 315.0573905601784190, -19.99999999999999289 ) ) ;
#3334 = ORIENTED_EDGE ( 'NONE', *, *, #14717, .T. ) ;
#3335 = CARTESIAN_POINT ( 'NONE',  ( -13.20868407381887444, 470.9948905683720000, -6.410867750099233042 ) ) ;
#3336 = EDGE_CURVE ( 'NONE', #264, #17635, #13237, .T. ) ;
#3337 = CARTESIAN_POINT ( 'NONE',  ( -45.43829269268869808, 284.1823905683720568, 3.332260488124734632 ) ) ;
#3338 = ORIENTED_EDGE ( 'NONE', *, *, #2723, .T. ) ;
#3339 = LINE ( 'NONE', #17436, #17978 ) ;
#3340 = CARTESIAN_POINT ( 'NONE',  ( -40.53162694259543031, 286.6198905683720000, 11.84573899990672885 ) ) ;
#3341 = AXIS2_PLACEMENT_3D ( 'NONE', #9961, #16580, #1768 ) ;
#3342 = CARTESIAN_POINT ( 'NONE',  ( -40.53162694259542320, 264.1198905683720568, -11.84573899990672707 ) ) ;
#3343 = CARTESIAN_POINT ( 'NONE',  ( -40.01497788969911795, 243.5573905765656377, 16.95518130045146776 ) ) ;
#3344 = CARTESIAN_POINT ( 'NONE',  ( -42.82802356641965247, 308.4948905601784759, 14.14213562373094923 ) ) ;
#3345 = CARTESIAN_POINT ( 'NONE',  ( -40.01497788969911795, 228.8073905601784759, 16.95518130045146776 ) ) ;
#3346 = CARTESIAN_POINT ( 'NONE',  ( -8.685887942688710339, 256.9948905765655809, -2.449293598294705724E-15 ) ) ;
#3347 = CARTESIAN_POINT ( 'NONE',  ( -44.16309181155855867, 263.2448905683720000, -6.410867750099231266 ) ) ;
#3348 = CARTESIAN_POINT ( 'NONE',  ( -19.19641293061498644, 371.9323905683720568, -14.20200298773971603 ) ) ;
#3349 = CARTESIAN_POINT ( 'NONE',  ( -43.63268616469407846, 200.3053519615658615, 1.302651870180923321 ) ) ;
#3350 = CARTESIAN_POINT ( 'NONE',  ( -48.68588794268872277, 461.9948905765656377, 0.000000000000000000 ) ) ;
#3351 = LINE ( 'NONE', #19784, #8741 ) ;
#3352 = ADVANCED_FACE ( 'NONE', ( #16590 ), #8347, .F. ) ;
#3353 = EDGE_CURVE ( 'NONE', #2858, #6356, #19494, .T. ) ;
#3354 = VECTOR ( 'NONE', #13359, 1000.000000000000000 ) ;
#3355 = CARTESIAN_POINT ( 'NONE',  ( -11.93348319268872793, 419.1823905683720000, -3.332260488124732856 ) ) ;
#3356 = CARTESIAN_POINT ( 'NONE',  ( -48.68588794268854514, 341.6823905765656946, -3.978247347593583783 ) ) ;
#3357 = ORIENTED_EDGE ( 'NONE', *, *, #13122, .F. ) ;
#3358 = CARTESIAN_POINT ( 'NONE',  ( -42.82802356641966668, 428.4948905601784759, 14.14213562373094923 ) ) ;
#3359 = VERTEX_POINT ( 'NONE', #2193 ) ;
#3360 = ORIENTED_EDGE ( 'NONE', *, *, #10816, .F. ) ;
#3361 = EDGE_LOOP ( 'NONE', ( #7885, #12101, #1111 ) ) ;
#3362 = FACE_BOUND ( 'NONE', #16513, .T. ) ;
#3363 = CARTESIAN_POINT ( 'NONE',  ( -45.64106924314017988, 296.3073905601784190, -11.32908994701042715 ) ) ;
#3364 = CARTESIAN_POINT ( 'NONE',  ( -46.31968306282883674, 303.6587712403113528, 33.59072564020503648 ) ) ;
#3365 = CARTESIAN_POINT ( 'NONE',  ( -42.88789093042843348, 346.3073905683720568, 9.489475012073734561 ) ) ;
#3366 = VECTOR ( 'NONE', #14553, 1000.000000000000000 ) ;
#3367 = VERTEX_POINT ( 'NONE', #3908 ) ;
#3368 = CARTESIAN_POINT ( 'NONE',  ( -32.66413529028189089, 484.1823905765656946, 19.99999999999999289 ) ) ;
#3369 = CARTESIAN_POINT ( 'NONE',  ( -40.53162694259543741, 365.1198905683720000, 11.84573899990672885 ) ) ;
#3370 = CARTESIAN_POINT ( 'NONE',  ( -3.959031995466599785E-15, 5.309483803148794756, 3.803704290982253156 ) ) ;
#3371 = CARTESIAN_POINT ( 'NONE',  ( -32.01814843081344719, 381.6823905683719431, -16.75240474999999307 ) ) ;
#3372 = EDGE_CURVE ( 'NONE', #7175, #6933, #7250, .T. ) ;
#3373 = CARTESIAN_POINT ( 'NONE',  ( -45.64106924314017988, 312.9323905765655809, 11.32908994701042715 ) ) ;
#3374 = CARTESIAN_POINT ( 'NONE',  ( -40.01497788969914637, 425.6823905601784759, -16.95518130045146421 ) ) ;
#3375 = CARTESIAN_POINT ( 'NONE',  ( -44.16309181155856578, 293.2448905683720000, -6.410867750099231266 ) ) ;
#3376 = CARTESIAN_POINT ( 'NONE',  ( 292.4526463419396691, 308.2087638784415162, -20.00000000000000355 ) ) ;
#3377 = CARTESIAN_POINT ( 'NONE',  ( -35.09675569278795138, 433.4948905683720568, -15.47720386886985544 ) ) ;
#3378 = CARTESIAN_POINT ( 'NONE',  ( -48.68588794268870146, 287.2448905601784759, 0.000000000000000000 ) ) ;
#3379 = CARTESIAN_POINT ( 'NONE',  ( -8.685887942688399477, 512.5573905601783053, -3.978247347592341221 ) ) ;
#3380 = DIRECTION ( 'NONE',  ( -1.000000000000000000, 0.000000000000000000, 0.000000000000000000 ) ) ;
#3381 = LINE ( 'NONE', #4885, #586 ) ;
#3382 = ADVANCED_FACE ( 'NONE', ( #1887, #15080 ), #17011, .T. ) ;
#3383 = CARTESIAN_POINT ( 'NONE',  ( -28.68588794268871212, 342.8698905683720000, -16.75240474999999307 ) ) ;
#3384 = CARTESIAN_POINT ( 'NONE',  ( -16.84014894278200458, 490.1198905683720000, -11.84573899990672707 ) ) ;
#3385 = ORIENTED_EDGE ( 'NONE', *, *, #14271, .T. ) ;
#3386 = CARTESIAN_POINT ( 'NONE',  ( -10.20829729246300133, 492.8698905601784759, -7.653668647301794969 ) ) ;
#3387 = CARTESIAN_POINT ( 'NONE',  ( -38.17536295476244845, 312.3073905683720000, -14.20200298773971426 ) ) ;
#3388 = ORIENTED_EDGE ( 'NONE', *, *, #13411, .T. ) ;
#3389 = CARTESIAN_POINT ( 'NONE',  ( -2.281271485192643599E-15, -5.469921996229795802, 3.525817189091422055 ) ) ;
#3390 = ORIENTED_EDGE ( 'NONE', *, *, #15256, .T. ) ;
#3391 = DIRECTION ( 'NONE',  ( 0.000000000000000000, 0.000000000000000000, -1.000000000000000000 ) ) ;
#3392 = SHAPE_REPRESENTATION ( 'Flywheel Manual Operating Handles', ( #12794 ), #16261 ) ;
#3393 = CARTESIAN_POINT ( 'NONE',  ( -13.20868407381886556, 400.9948905683720568, -6.410867750099233042 ) ) ;
#3394 = CARTESIAN_POINT ( 'NONE',  ( -28.68588794268872277, 444.4948905765655809, 19.99999999999999289 ) ) ;
#3395 = CARTESIAN_POINT ( 'NONE',  ( -35.09675569278795138, 421.9948905683720000, -15.47720386886985544 ) ) ;
#3396 = CARTESIAN_POINT ( 'NONE',  ( -45.43829269268872650, 453.8698905683720000, 0.000000000000000000 ) ) ;
#3397 = DIRECTION ( 'NONE',  ( 0.000000000000000000, -1.000000000000000000, 0.000000000000000000 ) ) ;
#3398 = CARTESIAN_POINT ( 'NONE',  ( -47.16347859291444422, 361.3698905765655809, -7.653668647301793193 ) ) ;
#3399 = CARTESIAN_POINT ( 'NONE',  ( -27.78321401995996709, 46.69440907075437508, 49.59323028521529153 ) ) ;
#3400 = CARTESIAN_POINT ( 'NONE',  ( -49.57497958038186425, 230.5765313837437418, -49.99999999999999289 ) ) ;
#3401 = CARTESIAN_POINT ( 'NONE',  ( -8.685887942688729879, 426.9948905765656377, -2.449293598294705724E-15 ) ) ;
#3402 = CARTESIAN_POINT ( 'NONE',  ( -24.70764059509557597, 489.1823905765656377, -19.99999999999999289 ) ) ;
#3403 = CARTESIAN_POINT ( 'NONE',  ( -42.88789093042844769, 504.4323905683721136, -9.489475012073736337 ) ) ;
#3404 = CARTESIAN_POINT ( 'NONE',  ( -28.68588794268874409, 608.2448905601786464, 0.000000000000000000 ) ) ;
#3405 = CARTESIAN_POINT ( 'NONE',  ( 81.24038404635965094, 30.52886280891152282, -131.1729372809869005 ) ) ;
#3406 = CARTESIAN_POINT ( 'NONE',  ( -36.33955658999052218, 419.1198905601784759, 18.47759065022572500 ) ) ;
#3407 = CARTESIAN_POINT ( 'NONE',  ( -35.09675569278795848, 417.2448905683720568, 15.47720386886985366 ) ) ;
#3408 = EDGE_CURVE ( 'NONE', #19361, #13635, #2087, .T. ) ;
#3409 = CARTESIAN_POINT ( 'NONE',  ( -16.84014894278196905, 229.1198905683720000, 11.84573899990672530 ) ) ;
#3410 = CARTESIAN_POINT ( 'NONE',  ( -13.20868407381886023, 359.4948905683720000, -6.410867750099233042 ) ) ;
#3411 = VECTOR ( 'NONE', #7075, 1000.000000000000000 ) ;
#3412 = EDGE_CURVE ( 'NONE', #8722, #8747, #574, .T. ) ;
#3413 = VERTEX_POINT ( 'NONE', #684 ) ;
#3414 = CARTESIAN_POINT ( 'NONE',  ( -14.48388495494901740, 519.8073905683720568, -9.489475012073736337 ) ) ;
#3415 = ORIENTED_EDGE ( 'NONE', *, *, #8284, .T. ) ;
#3416 = CARTESIAN_POINT ( 'NONE',  ( -19.19641293061499354, 441.9323905683720568, -14.20200298773971603 ) ) ;
#3417 = CARTESIAN_POINT ( 'NONE',  ( -22.27502019258949417, 516.9948905683720568, 15.47720386886985189 ) ) ;
#3418 = ORIENTED_EDGE ( 'NONE', *, *, #17690, .T. ) ;
#3419 = FACE_OUTER_BOUND ( 'NONE', #13096, .T. ) ;
#3420 = CARTESIAN_POINT ( 'NONE',  ( -11.93348319268873681, 488.5573905683720568, 3.332260488124728415 ) ) ;
#3421 = VERTEX_POINT ( 'NONE', #8777 ) ;
#3422 = CARTESIAN_POINT ( 'NONE',  ( -14.48388495494901562, 509.8073905683720000, -9.489475012073734561 ) ) ;
#3423 = CARTESIAN_POINT ( 'NONE',  ( -16.60355223547259484, 46.82116177588022765, -48.10739902922093592 ) ) ;
#3424 = CARTESIAN_POINT ( 'NONE',  ( -24.70764059509555821, 414.8073905765656946, 19.99999999999998934 ) ) ;
#3425 = CARTESIAN_POINT ( 'NONE',  ( -48.68588794268870146, 301.9948905765655809, 0.000000000000000000 ) ) ;
#3426 = CARTESIAN_POINT ( 'NONE',  ( -17.35679799567828496, 330.6823905601785896, 16.95518130045146421 ) ) ;
#3427 = DIRECTION ( 'NONE',  ( -1.191790137725560488E-16, 1.000000000000000000, -0.000000000000000000 ) ) ;
#3428 = LINE ( 'NONE', #10323, #5964 ) ;
#3429 = CARTESIAN_POINT ( 'NONE',  ( -33.84809828339280102, 56.85652257517428865, 49.33155846391706945 ) ) ;
#3430 = VECTOR ( 'NONE', #912, 1000.000000000000114 ) ;
#3431 = CARTESIAN_POINT ( 'NONE',  ( 30.42502041961813575, 271.1055109169419097, 20.00000000000000355 ) ) ;
#3432 = CARTESIAN_POINT ( 'NONE',  ( -32.01814843081344009, 297.5573905683720000, 16.75240474999999307 ) ) ;
#3433 = DIRECTION ( 'NONE',  ( -1.191790137725560488E-16, 1.000000000000000000, -0.000000000000000000 ) ) ;
#3434 = CARTESIAN_POINT ( 'NONE',  ( -48.68588794268869435, 267.5573905601784759, 3.978247347593168115 ) ) ;
#3435 = CARTESIAN_POINT ( 'NONE',  ( -45.64106924314018698, 412.9323905765655809, 11.32908994701042538 ) ) ;
#3436 = CARTESIAN_POINT ( 'NONE',  ( -13.20868407381884957, 289.7448905683720568, 6.410867750099229490 ) ) ;
#3437 = CYLINDRICAL_SURFACE ( 'NONE', #12222, 200.0000000000000000 ) ;
#3438 = CARTESIAN_POINT ( 'NONE',  ( -45.43829269268872650, 505.3698905683721136, 0.000000000000000000 ) ) ;
#3439 = AXIS2_PLACEMENT_3D ( 'NONE', #17420, #15482, #19038 ) ;
#3440 = ORIENTED_EDGE ( 'NONE', *, *, #8077, .T. ) ;
#3441 = CARTESIAN_POINT ( 'NONE',  ( -14.48388495494901385, 471.3073905683720568, -9.489475012073736337 ) ) ;
#3442 = CARTESIAN_POINT ( 'NONE',  ( -28.68588794268872633, 378.8848358243226357, 0.000000000000000000 ) ) ;
#3443 = CARTESIAN_POINT ( 'NONE',  ( -40.53162694259542320, 265.1198905683720568, 11.84573899990672885 ) ) ;
#3444 = EDGE_LOOP ( 'NONE', ( #12402, #11887, #11784, #15491 ) ) ;
#3445 = LINE ( 'NONE', #322, #5917 ) ;
#3446 = CARTESIAN_POINT ( 'NONE',  ( -16.84014894278197971, 261.6198905683720568, -11.84573899990672707 ) ) ;
#3447 = CARTESIAN_POINT ( 'NONE',  ( -48.68588794268869435, 252.3073905765655809, 3.978247347593168115 ) ) ;
#3448 = CARTESIAN_POINT ( 'NONE',  ( -41.83569717483972994, 135.1716627696692683, -24.99999999999998934 ) ) ;
#3449 = CARTESIAN_POINT ( 'NONE',  ( -45.64106924314017277, 228.1823905601784759, 11.32908994701042715 ) ) ;
#3450 = CARTESIAN_POINT ( 'NONE',  ( -11.73070664223723725, 257.9323905765656377, -11.32908994701042538 ) ) ;
#3451 = CARTESIAN_POINT ( 'NONE',  ( -25.35362745456396993, 266.6823905683720568, 16.75240474999998952 ) ) ;
#3452 = CARTESIAN_POINT ( 'NONE',  ( -35.09675569278795138, 357.2448905683720000, 15.47720386886985366 ) ) ;
#3453 = CARTESIAN_POINT ( 'NONE',  ( 5.074999999999999289, 0.000000000000000000, 0.000000000000000000 ) ) ;
#3454 = EDGE_CURVE ( 'NONE', #1161, #2785, #1691, .T. ) ;
#3455 = CARTESIAN_POINT ( 'NONE',  ( -44.16309181155857289, 424.4948905683720568, 6.410867750099241924 ) ) ;
#3456 = DIRECTION ( 'NONE',  ( -0.3505116388060184329, 0.000000000000000000, 0.9365583756827543516 ) ) ;
#3457 = ORIENTED_EDGE ( 'NONE', *, *, #19817, .T. ) ;
#3458 = CARTESIAN_POINT ( 'NONE',  ( -47.16347859291445133, 397.8698905601784759, 7.653668647301805628 ) ) ;
#3459 = EDGE_LOOP ( 'NONE', ( #14362, #5481, #21306, #3548, #4004, #4975 ) ) ;
#3460 = EDGE_LOOP ( 'NONE', ( #1257, #820, #12694, #3088 ) ) ;
#3461 = ORIENTED_EDGE ( 'NONE', *, *, #6048, .T. ) ;
#3462 = CARTESIAN_POINT ( 'NONE',  ( -25.35362745456400191, 528.1823905683719431, 16.75240474999998952 ) ) ;
#3463 = CARTESIAN_POINT ( 'NONE',  ( -8.685887942688715668, 301.9323905601784190, 3.978247347593161010 ) ) ;
#3464 = DIRECTION ( 'NONE',  ( 9.855701800883827197E-17, -1.000000000000000000, 0.000000000000000000 ) ) ;
#3465 = CARTESIAN_POINT ( 'NONE',  ( -32.01814843081344009, 323.1823905683720000, -16.75240474999999307 ) ) ;
#3466 = ORIENTED_EDGE ( 'NONE', *, *, #20411, .F. ) ;
#3467 = CARTESIAN_POINT ( 'NONE',  ( -32.66413529028189089, 489.8073905765656377, -19.99999999999999289 ) ) ;
#3468 = CARTESIAN_POINT ( 'NONE',  ( -19.19641293061498288, 357.3073905683720568, 14.20200298773971426 ) ) ;
#3469 = CARTESIAN_POINT ( 'NONE',  ( -35.09675569278794427, 361.9948905683720568, -15.47720386886985544 ) ) ;
#3470 = ADVANCED_FACE ( 'NONE', ( #13447 ), #3598, .F. ) ;
#3471 = VECTOR ( 'NONE', #2646, 1000.000000000000000 ) ;
#3472 = CARTESIAN_POINT ( 'NONE',  ( -24.70764059509555466, 299.1823905765656377, -19.99999999999999289 ) ) ;
#3473 = LINE ( 'NONE', #18600, #1719 ) ;
#3474 = CARTESIAN_POINT ( 'NONE',  ( -45.43829269268870519, 273.5573905683720000, -3.332260488124726638 ) ) ;
#3475 = DIRECTION ( 'NONE',  ( 0.000000000000000000, 1.000000000000000000, 0.000000000000000000 ) ) ;
#3476 = CARTESIAN_POINT ( 'NONE',  ( -45.43829269268871940, 425.3698905683720568, 0.000000000000000000 ) ) ;
#3477 = DIRECTION ( 'NONE',  ( -1.191790137725560488E-16, 1.000000000000000000, -0.000000000000000000 ) ) ;
#3478 = CARTESIAN_POINT ( 'NONE',  ( -36.33955658999052929, 515.3698905601784190, -18.47759065022572855 ) ) ;
#3479 = CARTESIAN_POINT ( 'NONE',  ( 4.700000000000000178, 0.000000000000000000, 0.000000000000000000 ) ) ;
#3480 = DIRECTION ( 'NONE',  ( -1.000000000000000000, 0.000000000000000000, 0.000000000000000000 ) ) ;
#3481 = CARTESIAN_POINT ( 'NONE',  ( -38.17536295476244135, 326.9323905683720568, 14.20200298773971781 ) ) ;
#3482 = CARTESIAN_POINT ( 'NONE',  ( -44.16309181155858710, 483.2448905683720000, -6.410867750099231266 ) ) ;
#3483 = ORIENTED_EDGE ( 'NONE', *, *, #11940, .F. ) ;
#3484 = CARTESIAN_POINT ( 'NONE',  ( -8.685887942688736985, 481.9323905601784759, 3.978247347593161010 ) ) ;
#3485 = CARTESIAN_POINT ( 'NONE',  ( -42.88789093042842637, 304.8073905683720000, 9.489475012073736337 ) ) ;
#3486 = ADVANCED_FACE ( 'NONE', ( #10499 ), #20149, .T. ) ;
#3487 = ORIENTED_EDGE ( 'NONE', *, *, #13735, .F. ) ;
#3488 =( GEOMETRIC_REPRESENTATION_CONTEXT ( 3 ) GLOBAL_UNCERTAINTY_ASSIGNED_CONTEXT ( ( #13089 ) ) GLOBAL_UNIT_ASSIGNED_CONTEXT ( ( #13667, #8565, #20256 ) ) REPRESENTATION_CONTEXT ( 'NONE', 'WORKASPACE' ) );
#3489 = AXIS2_PLACEMENT_3D ( 'NONE', #16687, #4772, #16792 ) ;
#3490 = CARTESIAN_POINT ( 'NONE',  ( -11.73070664223724613, 346.0573905765656377, 11.32908994701042005 ) ) ;
#3491 = ORIENTED_EDGE ( 'NONE', *, *, #4797, .F. ) ;
#3492 = CARTESIAN_POINT ( 'NONE',  ( 5.674999999999999822, 7.505553499465139389, 0.000000000000000000 ) ) ;
#3493 = CARTESIAN_POINT ( 'NONE',  ( -13.20868407381886556, 410.9948905683720000, -6.410867750099233042 ) ) ;
#3494 = CARTESIAN_POINT ( 'NONE',  ( -32.66413529028186957, 384.1823905765656377, 19.99999999999999289 ) ) ;
#3495 = CARTESIAN_POINT ( 'NONE',  ( -44.16309181155857289, 414.4948905683720000, 6.410867750099241924 ) ) ;
#3496 = CARTESIAN_POINT ( 'NONE',  ( -11.93348319268871016, 260.6823905683720000, -3.332260488124732856 ) ) ;
#3497 = CARTESIAN_POINT ( 'NONE',  ( -13.20868407381886911, 448.2448905683720000, 6.410867750099229490 ) ) ;
#3498 = SHAPE_DEFINITION_REPRESENTATION ( #16340, #18847 ) ;
#3499 = CYLINDRICAL_SURFACE ( 'NONE', #2527, 50.00000000000000000 ) ;
#3500 = EDGE_CURVE ( 'NONE', #6477, #2589, #5216, .T. ) ;
#3501 = CARTESIAN_POINT ( 'NONE',  ( -48.68588794268870856, 371.6823905765656377, -3.978247347593158345 ) ) ;
#3502 = DIRECTION ( 'NONE',  ( 0.000000000000000000, 1.000000000000000000, 0.000000000000000000 ) ) ;
#3503 = CARTESIAN_POINT ( 'NONE',  ( -8.685887942688532704, 262.5573905601784190, -3.978247347592740013 ) ) ;
#3504 = CARTESIAN_POINT ( 'NONE',  ( -11.93348319268871727, 328.5573905683720568, 3.332260488124728859 ) ) ;
#3505 = CARTESIAN_POINT ( 'NONE',  ( 88.28695088269886071, 142.5259582928263455, -20.00000000000000355 ) ) ;
#3506 = CARTESIAN_POINT ( 'NONE',  ( -45.43829269268871940, 505.0573905683721136, -3.332260488124726194 ) ) ;
#3507 = CARTESIAN_POINT ( 'NONE',  ( -22.62331590640576096, 213.9102039777116602, -11.80838889663596447 ) ) ;
#3508 = CARTESIAN_POINT ( 'NONE',  ( -36.33955658999052218, 465.3698905601784759, -18.47759065022572855 ) ) ;
#3509 = CARTESIAN_POINT ( 'NONE',  ( -48.68588794268873698, 573.2448905601785327, 0.000000000000000000 ) ) ;
#3510 = CARTESIAN_POINT ( 'NONE',  ( -22.27502019258947996, 398.4948905683720000, 15.47720386886985189 ) ) ;
#3511 = FACE_OUTER_BOUND ( 'NONE', #8929, .T. ) ;
#3512 =( BOUNDED_CURVE ( )  B_SPLINE_CURVE ( 2, ( #1201, #17730, #6257, #1618, #9715, #2924, #13192, #7979, #1298, #7771, #7872, #16336, #14501, #12971, #6361, #8191, #21084 ),
 .UNSPECIFIED., .F., .T. ) 
 B_SPLINE_CURVE_WITH_KNOTS ( ( 3, 2, 2, 2, 2, 2, 2, 2, 3 ),
 ( 0.1875000000000001665, 0.1894531250000001665, 0.1914062500000001665, 0.1933593750000001665, 0.1953125000000001665, 0.1972656250000001665, 0.1992187500000001665, 0.2011718750000001665, 0.2031250000000001665 ),
 .UNSPECIFIED. ) 
 CURVE ( )  GEOMETRIC_REPRESENTATION_ITEM ( )  RATIONAL_B_SPLINE_CURVE ( ( 0.9999999999999983347, 0.9807852804032320959, 1.000000000000000000, 0.9807852804032304306, 1.000000000000000000, 0.9807852804032304306, 1.000000000000000000, 0.9807852804032304306, 1.000000000000000000, 0.9807852804032304306, 1.000000000000000000, 0.9807852804032304306, 1.000000000000000000, 0.9807852804032304306, 1.000000000000000000, 0.9807852804032287652, 1.000000000000001554 ) ) 
 REPRESENTATION_ITEM ( '' )  );
#3513 = CARTESIAN_POINT ( 'NONE',  ( -20.29730442470228624, 222.0357903062241860, -14.50085278421890322 ) ) ;
#3514 = CARTESIAN_POINT ( 'NONE',  ( -22.27502019258948707, 370.7448905683720568, -15.47720386886985544 ) ) ;
#3515 = VERTEX_POINT ( 'NONE', #15498 ) ;
#3516 = CARTESIAN_POINT ( 'NONE',  ( -32.01814843081346851, 516.0573905683720568, 16.75240474999999307 ) ) ;
#3517 = ORIENTED_EDGE ( 'NONE', *, *, #18529, .F. ) ;
#3518 = CARTESIAN_POINT ( 'NONE',  ( -42.88789093042844058, 446.3073905683720568, 9.489475012073734561 ) ) ;
#3519 = CARTESIAN_POINT ( 'NONE',  ( -32.01814843081346851, 521.6823905683720568, -16.75240474999999307 ) ) ;
#3520 = EDGE_LOOP ( 'NONE', ( #13660, #20073 ) ) ;
#3521 = CIRCLE ( 'NONE', #13193, 4.000000000000001776 ) ;
#3522 = CARTESIAN_POINT ( 'NONE',  ( -28.68588794268873698, 529.4948905765655809, -19.99999999999999289 ) ) ;
#3523 = CARTESIAN_POINT ( 'NONE',  ( -44.16309181155857999, 484.4948905683720000, 6.410867750099241924 ) ) ;
#3524 = AXIS2_PLACEMENT_3D ( 'NONE', #11422, #7749, #3004 ) ;
#3525 = ORIENTED_EDGE ( 'NONE', *, *, #18276, .T. ) ;
#3526 = CARTESIAN_POINT ( 'NONE',  ( -48.68588794268872277, 487.2448905601784759, 0.000000000000000000 ) ) ;
#3527 = CARTESIAN_POINT ( 'NONE',  ( -40.01497788969914637, 430.4323905765655809, -16.95518130045146421 ) ) ;
#3528 = CARTESIAN_POINT ( 'NONE',  ( 107.6674317086782935, 187.4856410316723441, 20.00000000000000355 ) ) ;
#3529 = FACE_OUTER_BOUND ( 'NONE', #3176, .T. ) ;
#3530 = CARTESIAN_POINT ( 'NONE',  ( 157.1741849360543313, 610.7448905601785327, -9.864615503757139692 ) ) ;
#3531 = CARTESIAN_POINT ( 'NONE',  ( -48.68588794268872277, 471.9948905765656377, 0.000000000000000000 ) ) ;
#3532 = ADVANCED_FACE ( 'NONE', ( #1991 ), #18720, .F. ) ;
#3533 = PLANE ( 'NONE',  #849 ) ;
#3534 = DIRECTION ( 'NONE',  ( 1.000000000000000000, 0.000000000000000000, 0.000000000000000000 ) ) ;
#3535 = CARTESIAN_POINT ( 'NONE',  ( -43.68588794268869435, 200.1437886375728965, -2.037320803886357560E-15 ) ) ;
#3536 = CARTESIAN_POINT ( 'NONE',  ( -22.27502019258946930, 288.4948905683720000, 15.47720386886985189 ) ) ;
#3537 = CARTESIAN_POINT ( 'NONE',  ( -21.03221929538690915, 234.1198905601784475, -18.47759065022572855 ) ) ;
#3538 = CARTESIAN_POINT ( 'NONE',  ( -14.54375231895775578, 270.9948905601784759, 14.14213562373094568 ) ) ;
#3539 = DIRECTION ( 'NONE',  ( 1.000000000000000000, 0.000000000000000000, 0.000000000000000000 ) ) ;
#3540 = AXIS2_PLACEMENT_3D ( 'NONE', #6271, #3041, #19475 ) ;
#3541 = CARTESIAN_POINT ( 'NONE',  ( -11.93348319268871016, 280.3698905683720000, -2.051577885510841163E-15 ) ) ;
#3542 = EDGE_CURVE ( 'NONE', #16754, #11704, #13661, .T. ) ;
#3543 = ORIENTED_EDGE ( 'NONE', *, *, #15578, .T. ) ;
#3544 = DIRECTION ( 'NONE',  ( 0.000000000000000000, -1.000000000000000000, 0.000000000000000000 ) ) ;
#3545 = CARTESIAN_POINT ( 'NONE',  ( -11.93348319268873858, 500.0573905683720568, 3.332260488124728859 ) ) ;
#3546 = ADVANCED_FACE ( 'NONE', ( #12133 ), #18103, .T. ) ;
#3547 = ADVANCED_FACE ( 'NONE', ( #17120 ), #20248, .T. ) ;
#3548 = ORIENTED_EDGE ( 'NONE', *, *, #13562, .F. ) ;
#3549 = CARTESIAN_POINT ( 'NONE',  ( -11.93348319268873325, 460.6823905683720568, -3.332260488124732856 ) ) ;
#3550 = CARTESIAN_POINT ( 'NONE',  ( -38.17536295476243424, 265.4323905683720568, 14.20200298773971781 ) ) ;
#3551 = CIRCLE ( 'NONE', #16341, 175.0000000000000284 ) ;
#3552 = ORIENTED_EDGE ( 'NONE', *, *, #6959, .F. ) ;
#3553 = CARTESIAN_POINT ( 'NONE',  ( -41.83569717483972994, 303.6587712403113528, 25.00000000000000000 ) ) ;
#3554 = CARTESIAN_POINT ( 'NONE',  ( -19.19641293061496867, 251.9323905683720284, -14.20200298773971603 ) ) ;
#3555 = EDGE_CURVE ( 'NONE', #18299, #2963, #18614, .T. ) ;
#3556 = CARTESIAN_POINT ( 'NONE',  ( -45.64106924314017277, 252.9323905765656377, 11.32908994701042715 ) ) ;
#3557 = CARTESIAN_POINT ( 'NONE',  ( 0.000000000000000000, 0.000000000000000000, 0.000000000000000000 ) ) ;
#3558 = CARTESIAN_POINT ( 'NONE',  ( -48.68588794268869435, 226.9323905601785043, -3.978247347593158345 ) ) ;
#3559 = CARTESIAN_POINT ( 'NONE',  ( -13.20868407381884779, 258.2448905683720000, 6.410867750099229490 ) ) ;
#3560 = CARTESIAN_POINT ( 'NONE',  ( -45.43829269268870519, 365.6823905683720568, 3.332260488124734632 ) ) ;
#3561 = CARTESIAN_POINT ( 'NONE',  ( -8.685887942688742314, 573.2448905601785327, 2.449293598294706119E-15 ) ) ;
#3562 = VECTOR ( 'NONE', #14190, 1000.000000000000000 ) ;
#3563 = CARTESIAN_POINT ( 'NONE',  ( -44.16309181155857289, 404.4948905683720000, 6.410867750099241924 ) ) ;
#3564 = CARTESIAN_POINT ( 'NONE',  ( -40.01497788969915348, 508.8073905601784190, 16.95518130045146776 ) ) ;
#3565 = ORIENTED_EDGE ( 'NONE', *, *, #17674, .T. ) ;
#3566 = CARTESIAN_POINT ( 'NONE',  ( -11.73070664223725146, 401.3073905601784759, 11.32908994701042005 ) ) ;
#3567 = VERTEX_POINT ( 'NONE', #5738 ) ;
#3568 = ORIENTED_EDGE ( 'NONE', *, *, #10003, .F. ) ;
#3569 = ORIENTED_EDGE ( 'NONE', *, *, #8372, .T. ) ;
#3570 = CARTESIAN_POINT ( 'NONE',  ( -42.88789093042845479, 526.3073905683720568, 9.489475012073736337 ) ) ;
#3571 = CARTESIAN_POINT ( 'NONE',  ( -21.03221929538691626, 294.1198905601785327, -18.47759065022572855 ) ) ;
#3572 = CARTESIAN_POINT ( 'NONE',  ( -43.68588794268869435, 210.1437886375729533, -0.1639321870911867873 ) ) ;
#3573 = AXIS2_PLACEMENT_3D ( 'NONE', #764, #15580, #2590 ) ;
#3574 = CARTESIAN_POINT ( 'NONE',  ( -25.35362745456398770, 332.5573905683719431, -16.75240474999999307 ) ) ;
#3575 = VERTEX_POINT ( 'NONE', #4445 ) ;
#3576 = CARTESIAN_POINT ( 'NONE',  ( -32.01814843081344719, 371.6823905683720000, -16.75240474999999307 ) ) ;
#3577 = CARTESIAN_POINT ( 'NONE',  ( -40.53162694259543741, 375.1198905683720000, 11.84573899990672885 ) ) ;
#3578 = CARTESIAN_POINT ( 'NONE',  ( -36.33955658999050797, 303.8698905765656377, 18.47759065022572500 ) ) ;
#3579 = CARTESIAN_POINT ( 'NONE',  ( -10.76731745429009912, 56.85652257517428865, -118.3724535612433328 ) ) ;
#3580 = CARTESIAN_POINT ( 'NONE',  ( -11.93348319268870839, 259.1823905683720568, -3.332260488124732856 ) ) ;
#3581 = CARTESIAN_POINT ( 'NONE',  ( -42.82802356641966668, 438.4948905601784759, 14.14213562373094923 ) ) ;
#3582 = CARTESIAN_POINT ( 'NONE',  ( -45.43829269268871229, 425.6823905683720568, 3.332260488124734632 ) ) ;
#3583 = CARTESIAN_POINT ( 'NONE',  ( -29.89856342657186872, 48.13176998328706446, 121.3728849402414198 ) ) ;
#3584 = CARTESIAN_POINT ( 'NONE',  ( 158.8141120573112630, 610.7448905601785327, -10.00000000000000888 ) ) ;
#3585 = CARTESIAN_POINT ( 'NONE',  ( -18.68588794268873698, 281.1055109169419666, -40.00000000000000000 ) ) ;
#3586 = PRODUCT_DEFINITION_CONTEXT ( 'detailed design', #11918, 'design' ) ;
#3587 = CARTESIAN_POINT ( 'NONE',  ( -17.35679799567829562, 410.6823905601784759, 16.95518130045146421 ) ) ;
#3588 = CARTESIAN_POINT ( 'NONE',  ( -13.20868407381885490, 329.7448905683720568, 6.410867750099229490 ) ) ;
#3589 = CARTESIAN_POINT ( 'NONE',  ( -11.93348319268873503, 479.1823905683721136, -3.332260488124732856 ) ) ;
#3590 = ORIENTED_EDGE ( 'NONE', *, *, #16291, .T. ) ;
#3591 = CARTESIAN_POINT ( 'NONE',  ( -32.66413529028189089, 475.0573905601785327, -19.99999999999999289 ) ) ;
#3592 = CARTESIAN_POINT ( 'NONE',  ( -42.88789093042842637, 302.9323905683720568, -9.489475012073736337 ) ) ;
#3593 = VECTOR ( 'NONE', #4192, 1000.000000000000000 ) ;
#3594 = EDGE_CURVE ( 'NONE', #5825, #17823, #13934, .T. ) ;
#3595 = ORIENTED_EDGE ( 'NONE', *, *, #2237, .F. ) ;
#3596 = CARTESIAN_POINT ( 'NONE',  ( -21.03221929538690915, 345.1198905765656377, 18.47759065022572500 ) ) ;
#3597 = EDGE_LOOP ( 'NONE', ( #18467, #9370 ) ) ;
#3598 = PLANE ( 'NONE',  #6702 ) ;
#3599 = CARTESIAN_POINT ( 'NONE',  ( -13.20868407381886200, 380.9948905683720568, -6.410867750099233042 ) ) ;
#3600 = CARTESIAN_POINT ( 'NONE',  ( -45.64106924314019409, 478.1823905601785327, 11.32908994701042538 ) ) ;
#3601 = CARTESIAN_POINT ( 'NONE',  ( 0.000000000000000000, 610.7448905601785327, 0.000000000000000000 ) ) ;
#3602 = CARTESIAN_POINT ( 'NONE',  ( -14.48388495494900496, 427.9323905683720568, 9.489475012073732785 ) ) ;
#3603 = CARTESIAN_POINT ( 'NONE',  ( -40.53162694259542320, 266.6198905683720568, 11.84573899990672885 ) ) ;
#3604 = CARTESIAN_POINT ( 'NONE',  ( -40.53162694259544452, 435.1198905683720000, 11.84573899990672885 ) ) ;
#3605 = CARTESIAN_POINT ( 'NONE',  ( -8.685887942688742314, 573.2448905601785327, 2.449293598294706119E-15 ) ) ;
#3606 = CARTESIAN_POINT ( 'NONE',  ( -32.66413529028187668, 354.1823905765656377, 19.99999999999999289 ) ) ;
#3607 = FACE_OUTER_BOUND ( 'NONE', #17222, .T. ) ;
#3608 = DIRECTION ( 'NONE',  ( -1.191790137725560488E-16, 1.000000000000000000, -0.000000000000000000 ) ) ;
#3609 = CARTESIAN_POINT ( 'NONE',  ( -32.01814843081344009, 326.0573905683719431, 16.75240474999999307 ) ) ;
#3610 = DIRECTION ( 'NONE',  ( -1.000000000000000000, 0.000000000000000000, 0.000000000000000000 ) ) ;
#3611 = CARTESIAN_POINT ( 'NONE',  ( -19.19641293061499354, 468.8073905683720000, 14.20200298773971426 ) ) ;
#3612 = ADVANCED_FACE ( 'NONE', ( #12454 ), #18829, .F. ) ;
#3613 = CARTESIAN_POINT ( 'NONE',  ( -42.82802356641966668, 433.2448905765656377, 14.14213562373094923 ) ) ;
#3614 = SURFACE_STYLE_USAGE ( .BOTH. , #14988 ) ;
#3615 = CARTESIAN_POINT ( 'NONE',  ( -40.01497788969913927, 418.8073905601785896, 16.95518130045146776 ) ) ;
#3616 = CARTESIAN_POINT ( 'NONE',  ( -22.27502019258947996, 388.4948905683720000, 15.47720386886985189 ) ) ;
#3617 = DIRECTION ( 'NONE',  ( -3.836511174089486173E-16, 0.000000000000000000, 1.000000000000000000 ) ) ;
#3618 = CARTESIAN_POINT ( 'NONE',  ( -21.03221929538693047, 530.3698905601784190, 18.47759065022572500 ) ) ;
#3619 = CARTESIAN_POINT ( 'NONE',  ( -40.53162694259543741, 362.6198905683720000, -11.84573899990672707 ) ) ;
#3620 = EDGE_CURVE ( 'NONE', #18564, #7989, #17080, .T. ) ;
#3621 = ORIENTED_EDGE ( 'NONE', *, *, #7962, .F. ) ;
#3622 = EDGE_CURVE ( 'NONE', #5930, #5058, #4011, .T. ) ;
#3623 = CARTESIAN_POINT ( 'NONE',  ( -45.43829269268872650, 524.1823905683720568, 3.332260488124734632 ) ) ;
#3624 = ORIENTED_EDGE ( 'NONE', *, *, #5125, .T. ) ;
#3625 = CARTESIAN_POINT ( 'NONE',  ( -42.88789093042844058, 436.3073905683720568, 9.489475012073734561 ) ) ;
#3626 = CARTESIAN_POINT ( 'NONE',  ( -14.48388495494901740, 527.9323905683719431, 9.489475012073732785 ) ) ;
#3627 = ORIENTED_EDGE ( 'NONE', *, *, #3372, .T. ) ;
#3628 = CARTESIAN_POINT ( 'NONE',  ( -165.7253922195052951, 600.7448905601785327, 108.8355377051282176 ) ) ;
#3629 = CARTESIAN_POINT ( 'NONE',  ( -42.88789093042844769, 484.8073905683720000, 9.489475012073736337 ) ) ;
#3630 = ORIENTED_EDGE ( 'NONE', *, *, #19803, .T. ) ;
#3631 = CARTESIAN_POINT ( 'NONE',  ( -13.20868407381887444, 488.2448905683720000, 6.410867750099229490 ) ) ;
#3632 = CARTESIAN_POINT ( 'NONE',  ( -27.79598376143726668, 46.69101496124648065, -49.59521087409807905 ) ) ;
#3633 = CARTESIAN_POINT ( 'NONE',  ( -48.68588794268871567, 432.3073905765656946, 3.978247347593168115 ) ) ;
#3634 = CYLINDRICAL_SURFACE ( 'NONE', #18254, 22.72497359561857877 ) ;
#3635 = CARTESIAN_POINT ( 'NONE',  ( 4.700000000000000178, 3.752776749732560368, -6.499999999999999112 ) ) ;
#3636 = CARTESIAN_POINT ( 'NONE',  ( -42.82802356641966668, 440.7448905765656377, -14.14213562373094746 ) ) ;
#3637 = CARTESIAN_POINT ( 'NONE',  ( 6.416697501590670427, 172.9933428177121471, -45.00000000000000000 ) ) ;
#3638 = EDGE_CURVE ( 'NONE', #9753, #5025, #10707, .T. ) ;
#3639 = CARTESIAN_POINT ( 'NONE',  ( -47.16347859291445133, 436.6198905601784759, -7.653668647301793193 ) ) ;
#3640 = CARTESIAN_POINT ( 'NONE',  ( -42.82802356641963826, 204.8148611821455916, -5.000000000000001776 ) ) ;
#3641 =( BOUNDED_CURVE ( )  B_SPLINE_CURVE ( 2, ( #10065, #14056, #3690, #18500, #6924, #13550, #9059, #10276, #5924, #2691, #17402, #12535, #2077, #15573, #20139, #360, #19129 ),
 .UNSPECIFIED., .F., .T. ) 
 B_SPLINE_CURVE_WITH_KNOTS ( ( 3, 2, 2, 2, 2, 2, 2, 2, 3 ),
 ( 0.7968750000000002220, 0.7988281250000002220, 0.8007812500000002220, 0.8027343750000002220, 0.8046875000000002220, 0.8066406250000002220, 0.8085937500000002220, 0.8105468750000002220, 0.8125000000000002220 ),
 .UNSPECIFIED. ) 
 CURVE ( )  GEOMETRIC_REPRESENTATION_ITEM ( )  RATIONAL_B_SPLINE_CURVE ( ( 0.9999999999999977796, 0.9807852804032326510, 1.000000000000000000, 0.9807852804032304306, 1.000000000000000000, 0.9807852804032304306, 1.000000000000000000, 0.9807852804032304306, 1.000000000000000000, 0.9807852804032304306, 1.000000000000000000, 0.9807852804032304306, 1.000000000000000000, 0.9807852804032304306, 1.000000000000000000, 0.9807852804032282101, 1.000000000000002220 ) ) 
 REPRESENTATION_ITEM ( '' )  );
#3642 = CARTESIAN_POINT ( 'NONE',  ( -45.43829269268870519, 305.3698905683720568, 0.000000000000000000 ) ) ;
#3643 = B_SPLINE_CURVE_WITH_KNOTS ( 'NONE', 3,
 ( #14939, #18270, #124, #3672, #16876, #6697 ),
 .UNSPECIFIED., .F., .F.,
 ( 4, 2, 4 ),
 ( 2.380733003136581732E-07, 0.001898835937927382655, 0.003797433802554451947 ),
 .UNSPECIFIED. ) ;
#3644 = CARTESIAN_POINT ( 'NONE',  ( 0.000000000000000000, 620.7448905601785327, 0.000000000000000000 ) ) ;
#3645 = CARTESIAN_POINT ( 'NONE',  ( -38.17536295476246266, 456.9323905683720000, 14.20200298773971781 ) ) ;
#3646 = CARTESIAN_POINT ( 'NONE',  ( -48.68588794268873698, 573.2448905601785327, 0.000000000000000000 ) ) ;
#3647 = CARTESIAN_POINT ( 'NONE',  ( -25.35362745456398414, 292.5573905683720568, -16.75240474999999307 ) ) ;
#3648 = ORIENTED_EDGE ( 'NONE', *, *, #4601, .F. ) ;
#3649 = CARTESIAN_POINT ( 'NONE',  ( -32.66413529028185536, 269.4323905601784759, 19.99999999999999289 ) ) ;
#3650 = CARTESIAN_POINT ( 'NONE',  ( -32.01814843081346140, 513.1823905683721705, -16.75240474999999307 ) ) ;
#3651 = ORIENTED_EDGE ( 'NONE', *, *, #13101, .T. ) ;
#3652 = CARTESIAN_POINT ( 'NONE',  ( -35.09675569278795848, 473.4948905683720000, -15.47720386886985544 ) ) ;
#3653 = DIRECTION ( 'NONE',  ( 1.000000000000000000, 0.000000000000000000, 0.000000000000000000 ) ) ;
#3654 = CARTESIAN_POINT ( 'NONE',  ( -25.35362745456398059, 261.0573905683720000, -16.75240474999999307 ) ) ;
#3655 = ORIENTED_EDGE ( 'NONE', *, *, #12335, .F. ) ;
#3656 = LINE ( 'NONE', #13404, #416 ) ;
#3657 = CARTESIAN_POINT ( 'NONE',  ( -13.20868407381884957, 270.9948905683720000, -6.410867750099233042 ) ) ;
#3658 = CARTESIAN_POINT ( 'NONE',  ( -38.17536295476243424, 236.9323905683720000, 14.20200298773971781 ) ) ;
#3659 = DIRECTION ( 'NONE',  ( -1.000000000000000000, -0.000000000000000000, -0.000000000000000000 ) ) ;
#3660 = DIRECTION ( 'NONE',  ( -0.000000000000000000, -0.000000000000000000, 1.000000000000000000 ) ) ;
#3661 = CARTESIAN_POINT ( 'NONE',  ( -35.09675569278793716, 265.7448905683720000, 15.47720386886985366 ) ) ;
#3662 = CARTESIAN_POINT ( 'NONE',  ( -28.68588794268871212, 347.8698905683720568, 16.75240474999999307 ) ) ;
#3663 = CARTESIAN_POINT ( 'NONE',  ( -28.68588794268875120, 610.7448905601785327, 0.000000000000000000 ) ) ;
#3664 = AXIS2_PLACEMENT_3D ( 'NONE', #7699, #2528, #16051 ) ;
#3665 = CARTESIAN_POINT ( 'NONE',  ( -11.93348319268872615, 408.5573905683720568, 3.332260488124728415 ) ) ;
#3666 = CARTESIAN_POINT ( 'NONE',  ( -8.685887942689081598, 511.9323905601784759, 3.978247347593985683 ) ) ;
#3667 = VERTEX_POINT ( 'NONE', #10605 ) ;
#3668 = CARTESIAN_POINT ( 'NONE',  ( -28.68588794268872277, 414.7448905601784759, -19.99999999999999289 ) ) ;
#3669 = EDGE_CURVE ( 'NONE', #9372, #16429, #796, .T. ) ;
#3670 = AXIS2_PLACEMENT_3D ( 'NONE', #15786, #15679, #13834 ) ;
#3671 = ORIENTED_EDGE ( 'NONE', *, *, #12063, .T. ) ;
#3672 = CARTESIAN_POINT ( 'NONE',  ( 0.05533025579362017138, 6.264553569211842365, -2.149474931388135612 ) ) ;
#3673 = ORIENTED_EDGE ( 'NONE', *, *, #14717, .F. ) ;
#3674 = ORIENTED_EDGE ( 'NONE', *, *, #18002, .F. ) ;
#3675 = CARTESIAN_POINT ( 'NONE',  ( -42.88789093042845479, 534.4323905683720568, -9.489475012073736337 ) ) ;
#3676 = CARTESIAN_POINT ( 'NONE',  ( -40.01497788969912506, 288.8073905601785327, 16.95518130045146776 ) ) ;
#3677 = CARTESIAN_POINT ( 'NONE',  ( 158.8141120573112630, 610.7448905601785327, 0.000000000000000000 ) ) ;
#3678 = CARTESIAN_POINT ( 'NONE',  ( -44.16309181155855867, 325.9948905683720000, 6.410867750099241924 ) ) ;
#3679 = ORIENTED_EDGE ( 'NONE', *, *, #2611, .T. ) ;
#3680 = CARTESIAN_POINT ( 'NONE',  ( -42.88789093042843348, 354.8073905683720568, 9.489475012073736337 ) ) ;
#3681 = CARTESIAN_POINT ( 'NONE',  ( -22.27502019258947641, 366.9948905683720568, 15.47720386886985189 ) ) ;
#3682 = AXIS2_PLACEMENT_3D ( 'NONE', #10869, #12826, #17475 ) ;
#3683 = CARTESIAN_POINT ( 'NONE',  ( -47.16347859291443712, 312.6198905765655809, 7.653668647301805628 ) ) ;
#3684 = CARTESIAN_POINT ( 'NONE',  ( -42.88789093042841927, 262.9323905683720568, -9.489475012073734561 ) ) ;
#3685 = CARTESIAN_POINT ( 'NONE',  ( -32.66413529028188378, 464.1823905765656377, 19.99999999999999289 ) ) ;
#3686 = CARTESIAN_POINT ( 'NONE',  ( -14.48388495494900496, 421.3073905683720000, -9.489475012073736337 ) ) ;
#3687 = VECTOR ( 'NONE', #20830, 1000.000000000000000 ) ;
#3688 = LINE ( 'NONE', #5304, #6453 ) ;
#3689 = CARTESIAN_POINT ( 'NONE',  ( -36.33955658999053639, 503.8698905765656377, 18.47759065022572500 ) ) ;
#3690 = CARTESIAN_POINT ( 'NONE',  ( -10.20829729246297646, 276.3698905765656377, 7.653668647301790529 ) ) ;
#3691 = CARTESIAN_POINT ( 'NONE',  ( -28.68588794268871212, 332.8698905683720000, -16.75240474999999307 ) ) ;
#3692 = CARTESIAN_POINT ( 'NONE',  ( -19.19641293061499709, 470.4323905683719431, -14.20200298773971603 ) ) ;
#3693 = ORIENTED_EDGE ( 'NONE', *, *, #17226, .F. ) ;
#3694 = CARTESIAN_POINT ( 'NONE',  ( -40.01497788969915348, 475.6823905601784190, -16.95518130045146421 ) ) ;
#3695 = CARTESIAN_POINT ( 'NONE',  ( -45.43829269268869808, 293.5573905683720568, -3.332260488124726194 ) ) ;
#3696 = VECTOR ( 'NONE', #19761, 1000.000000000000000 ) ;
#3697 = DIRECTION ( 'NONE',  ( 0.000000000000000000, 0.000000000000000000, 1.000000000000000000 ) ) ;
#3698 = ORIENTED_EDGE ( 'NONE', *, *, #1809, .T. ) ;
#3699 = DIRECTION ( 'NONE',  ( 0.000000000000000000, 0.000000000000000000, -1.000000000000000000 ) ) ;
#3700 = CARTESIAN_POINT ( 'NONE',  ( -42.88789093042843348, 384.4323905683720568, -9.489475012073734561 ) ) ;
#3701 = DIRECTION ( 'NONE',  ( -1.191790137725560488E-16, 1.000000000000000000, -0.000000000000000000 ) ) ;
#3702 = CARTESIAN_POINT ( 'NONE',  ( -48.68588794268870856, 381.9948905765655809, 0.000000000000000000 ) ) ;
#3703 = CARTESIAN_POINT ( 'NONE',  ( -28.68588794268872277, 431.3698905683720000, -16.75240474999999307 ) ) ;
#3704 = CARTESIAN_POINT ( 'NONE',  ( -44.16309181155855157, 265.9948905683720000, 6.410867750099241924 ) ) ;
#3705 = CARTESIAN_POINT ( 'NONE',  ( -13.20868407381886733, 419.4948905683720000, -6.410867750099233042 ) ) ;
#3706 = CARTESIAN_POINT ( 'NONE',  ( 0.000000000000000000, 0.000000000000000000, 0.000000000000000000 ) ) ;
#3707 = CARTESIAN_POINT ( 'NONE',  ( -48.68588794268870856, 361.6823905765656946, -3.978247347593158345 ) ) ;
#3708 = FACE_OUTER_BOUND ( 'NONE', #18774, .T. ) ;
#3709 = CARTESIAN_POINT ( 'NONE',  ( -25.35362745456398770, 321.0573905683720000, -16.75240474999999307 ) ) ;
#3710 = CARTESIAN_POINT ( 'NONE',  ( -8.685887942688742314, 573.2448905601785327, 2.449293598294706119E-15 ) ) ;
#3711 = CARTESIAN_POINT ( 'NONE',  ( -44.16309181155857999, 475.9948905683720000, 6.410867750099241924 ) ) ;
#3712 = VECTOR ( 'NONE', #411, 1000.000000000000000 ) ;
#3713 = CARTESIAN_POINT ( 'NONE',  ( 20.42502041961806825, 281.1055109169419666, -20.00000000000000355 ) ) ;
#3714 = DIRECTION ( 'NONE',  ( -1.000000000000000000, -0.000000000000000000, -0.000000000000000000 ) ) ;
#3715 = CARTESIAN_POINT ( 'NONE',  ( -42.82802356641965247, 305.9948905601784759, -14.14213562373094746 ) ) ;
#3716 = EDGE_CURVE ( 'NONE', #6455, #20328, #899, .T. ) ;
#3717 = VECTOR ( 'NONE', #20320, 1000.000000000000000 ) ;
#3718 = CARTESIAN_POINT ( 'NONE',  ( -45.43829269268871940, 395.3698905683720000, 0.000000000000000000 ) ) ;
#3719 = CARTESIAN_POINT ( 'NONE',  ( 6.416697501590670427, 172.9933428177121471, -50.00000000000000000 ) ) ;
#3720 = EDGE_CURVE ( 'NONE', #3882, #15977, #19085, .T. ) ;
#3721 = CARTESIAN_POINT ( 'NONE',  ( -14.54375231895778775, 530.9948905601784190, 14.14213562373094568 ) ) ;
#3722 = CARTESIAN_POINT ( 'NONE',  ( -32.01814843081344719, 356.0573905683719431, 16.75240474999999307 ) ) ;
#3723 = ORIENTED_EDGE ( 'NONE', *, *, #7317, .T. ) ;
#3724 = CARTESIAN_POINT ( 'NONE',  ( -14.48388495494901740, 527.9323905683719431, 9.489475012073732785 ) ) ;
#3725 = ORIENTED_EDGE ( 'NONE', *, *, #18225, .T. ) ;
#3726 = CARTESIAN_POINT ( 'NONE',  ( -45.43829269268872650, 523.5573905683721705, -3.332260488124726194 ) ) ;
#3727 = EDGE_LOOP ( 'NONE', ( #1724, #19469, #12666, #12427 ) ) ;
#3728 = CARTESIAN_POINT ( 'NONE',  ( -17.35679799567831338, 493.8073905601785327, -16.95518130045146421 ) ) ;
#3729 = CARTESIAN_POINT ( 'NONE',  ( -22.27502019258949062, 476.9948905683720000, 15.47720386886985189 ) ) ;
#3730 = VERTEX_POINT ( 'NONE', #17433 ) ;
#3731 = CARTESIAN_POINT ( 'NONE',  ( -28.68588794268873343, 491.3698905683720568, -16.75240474999999307 ) ) ;
#3732 = DIRECTION ( 'NONE',  ( 0.000000000000000000, -0.5000000000000004441, 0.8660254037844383745 ) ) ;
#3733 = CARTESIAN_POINT ( 'NONE',  ( -36.33955658999051508, 420.1198905765656377, -18.47759065022572855 ) ) ;
#3734 = DIRECTION ( 'NONE',  ( 0.3512089204514987073, 0.000000000000000000, -0.9362971185447986899 ) ) ;
#3735 = CARTESIAN_POINT ( 'NONE',  ( -48.68588794268874409, 548.2448905601784190, 2.449293598294706513E-15 ) ) ;
#3736 = DIRECTION ( 'NONE',  ( 1.000000000000000000, 0.000000000000000000, 0.000000000000000000 ) ) ;
#3737 = EDGE_CURVE ( 'NONE', #21308, #4925, #2504, .T. ) ;
#3738 = DIRECTION ( 'NONE',  ( -1.000000000000000000, 0.000000000000000000, 0.000000000000000000 ) ) ;
#3739 = DIRECTION ( 'NONE',  ( 0.000000000000000000, 1.000000000000000000, 0.000000000000000000 ) ) ;
#3740 = CARTESIAN_POINT ( 'NONE',  ( -38.17536295476244845, 303.8073905683720000, -14.20200298773971426 ) ) ;
#3741 = CIRCLE ( 'NONE', #12392, 49.60091809715359545 ) ;
#3742 = DIRECTION ( 'NONE',  ( 0.8090169943749474513, 0.000000000000000000, 0.5877852522924730261 ) ) ;
#3743 = CARTESIAN_POINT ( 'NONE',  ( -40.53162694259545162, 454.1198905683720568, -11.84573899990672707 ) ) ;
#3744 = CARTESIAN_POINT ( 'NONE',  ( -33.61217542136964909, 54.48747864393421736, -49.35581280498866619 ) ) ;
#3745 = CARTESIAN_POINT ( 'NONE',  ( -14.48388495494898720, 279.4323905683720568, 9.489475012073732785 ) ) ;
#3746 = ORIENTED_EDGE ( 'NONE', *, *, #20933, .T. ) ;
#3747 = FACE_OUTER_BOUND ( 'NONE', #10596, .T. ) ;
#3748 = CARTESIAN_POINT ( 'NONE',  ( -25.35362745456400901, 512.5573905683720568, -16.75240474999999307 ) ) ;
#3749 = ADVANCED_FACE ( 'NONE', ( #12570 ), #7358, .T. ) ;
#3750 = ORIENTED_EDGE ( 'NONE', *, *, #16376, .T. ) ;
#3751 = CARTESIAN_POINT ( 'NONE',  ( -16.84014894278199748, 459.1198905683720568, 11.84573899990672530 ) ) ;
#3752 = LINE ( 'NONE', #16860, #5533 ) ;
#3753 = CARTESIAN_POINT ( 'NONE',  ( -11.93348319268871016, 259.1823905683720000, -3.332260488124732856 ) ) ;
#3754 = EDGE_LOOP ( 'NONE', ( #11626, #9540 ) ) ;
#3755 = CARTESIAN_POINT ( 'NONE',  ( -36.33955658999051508, 333.8698905765656377, 18.47759065022572500 ) ) ;
#3756 = AXIS2_PLACEMENT_3D ( 'NONE', #6868, #20504, #8492 ) ;
#3757 = CARTESIAN_POINT ( 'NONE',  ( -11.73070664223724613, 307.9323905765656946, -11.32908994701042538 ) ) ;
#3758 = CARTESIAN_POINT ( 'NONE',  ( -42.88789093042841927, 236.3073905683720284, 9.489475012073734561 ) ) ;
#3759 =( BOUNDED_CURVE ( )  B_SPLINE_CURVE ( 2, ( #20392, #11953, #12281, #410, #12173, #3948, #18863, #13597, #20184, #8706, #2233, #4053, #8812, #18549, #10533, #16943, #15429 ),
 .UNSPECIFIED., .F., .T. ) 
 B_SPLINE_CURVE_WITH_KNOTS ( ( 3, 2, 2, 2, 2, 2, 2, 2, 3 ),
 ( 0.1718750000000001665, 0.1738281250000001665, 0.1757812500000001665, 0.1777343750000001665, 0.1796875000000001665, 0.1816406250000001665, 0.1835937500000001665, 0.1855468750000001665, 0.1875000000000001665 ),
 .UNSPECIFIED. ) 
 CURVE ( )  GEOMETRIC_REPRESENTATION_ITEM ( )  RATIONAL_B_SPLINE_CURVE ( ( 0.9999999999999983347, 0.9807852804032320959, 1.000000000000000000, 0.9807852804032304306, 1.000000000000000000, 0.9807852804032304306, 1.000000000000000000, 0.9807852804032304306, 1.000000000000000000, 0.9807852804032304306, 1.000000000000000000, 0.9807852804032304306, 1.000000000000000000, 0.9807852804032304306, 1.000000000000000000, 0.9807852804032287652, 1.000000000000001554 ) ) 
 REPRESENTATION_ITEM ( '' )  );
#3760 = ADVANCED_FACE ( 'NONE', ( #19052 ), #6061, .T. ) ;
#3761 = DIRECTION ( 'NONE',  ( -0.000000000000000000, -0.000000000000000000, -1.000000000000000000 ) ) ;
#3762 = CARTESIAN_POINT ( 'NONE',  ( -18.67110661049051146, 223.9107902980306335, -17.31196565581893765 ) ) ;
#3763 = DIRECTION ( 'NONE',  ( 0.000000000000000000, 0.000000000000000000, 1.000000000000000000 ) ) ;
#3764 = CARTESIAN_POINT ( 'NONE',  ( -42.88789093042841927, 244.8073905683720568, 9.489475012073736337 ) ) ;
#3765 = CARTESIAN_POINT ( 'NONE',  ( -44.16309181155857289, 364.7448905683720568, -6.410867750099231266 ) ) ;
#3766 = CARTESIAN_POINT ( 'NONE',  ( -36.33955658999050797, 279.1198905601784759, 18.47759065022572500 ) ) ;
#3767 = CIRCLE ( 'NONE', #15881, 9.999999999999994671 ) ;
#3768 = CARTESIAN_POINT ( 'NONE',  ( -19.19641293061498999, 400.4323905683720568, -14.20200298773971603 ) ) ;
#3769 = CARTESIAN_POINT ( 'NONE',  ( 30.42502041961814996, 180.1716627696692967, 40.00000000000000000 ) ) ;
#3770 = CARTESIAN_POINT ( 'NONE',  ( -32.66413529028188378, 415.0573905601785327, -19.99999999999999289 ) ) ;
#3771 = ORIENTED_EDGE ( 'NONE', *, *, #15494, .F. ) ;
#3772 = LINE ( 'NONE', #5608, #830 ) ;
#3773 = ORIENTED_EDGE ( 'NONE', *, *, #17514, .T. ) ;
#3774 = ORIENTED_EDGE ( 'NONE', *, *, #4850, .F. ) ;
#3775 = DIRECTION ( 'NONE',  ( -1.191790137725560488E-16, 1.000000000000000000, -0.000000000000000000 ) ) ;
#3776 = CARTESIAN_POINT ( 'NONE',  ( -24.70764059509553690, 280.0573905601784759, 19.99999999999998934 ) ) ;
#3777 = DIRECTION ( 'NONE',  ( 1.000000000000000000, 0.000000000000000000, 0.000000000000000000 ) ) ;
#3778 = CARTESIAN_POINT ( 'NONE',  ( -40.53162694259543031, 316.6198905683720568, 11.84573899990672885 ) ) ;
#3779 = CARTESIAN_POINT ( 'NONE',  ( -35.09675569278795138, 345.7448905683720568, 15.47720386886985366 ) ) ;
#3780 = CARTESIAN_POINT ( 'NONE',  ( -45.43829269268871229, 364.1823905683720568, 3.332260488124734632 ) ) ;
#3781 = AXIS2_PLACEMENT_3D ( 'NONE', #17934, #16438, #9815 ) ;
#3782 = CARTESIAN_POINT ( 'NONE',  ( -42.82802356641965247, 283.2448905765656377, 14.14213562373094923 ) ) ;
#3783 = DIRECTION ( 'NONE',  ( 0.000000000000000000, 0.000000000000000000, -1.000000000000000000 ) ) ;
#3784 = CARTESIAN_POINT ( 'NONE',  ( -32.01814843081344009, 276.0573905683720568, 16.75240474999999307 ) ) ;
#3785 = CARTESIAN_POINT ( 'NONE',  ( 88.28695088269886071, 142.5259582928263455, 40.00000000000000000 ) ) ;
#3786 = EDGE_CURVE ( 'NONE', #15417, #3359, #12531, .T. ) ;
#3787 = CARTESIAN_POINT ( 'NONE',  ( -14.48388495494900496, 419.4323905683720568, 9.489475012073732785 ) ) ;
#3788 = ADVANCED_FACE ( 'NONE', ( #2832 ), #14605, .F. ) ;
#3789 = DIRECTION ( 'NONE',  ( -1.191790137725560488E-16, 1.000000000000000000, -0.000000000000000000 ) ) ;
#3790 = CARTESIAN_POINT ( 'NONE',  ( -21.03221929538692692, 505.1198905765656946, 18.47759065022572500 ) ) ;
#3791 = LINE ( 'NONE', #10277, #14282 ) ;
#3792 = CARTESIAN_POINT ( 'NONE',  ( -42.88789093042842637, 326.3073905683721136, 9.489475012073736337 ) ) ;
#3793 = CARTESIAN_POINT ( 'NONE',  ( -35.09675569278795848, 461.9948905683720000, -15.47720386886985544 ) ) ;
#3794 = ORIENTED_EDGE ( 'NONE', *, *, #5782, .T. ) ;
#3795 = CARTESIAN_POINT ( 'NONE',  ( -42.82802356641967378, 468.4948905601785327, 14.14213562373094923 ) ) ;
#3796 = CARTESIAN_POINT ( 'NONE',  ( -35.09675569278793716, 291.9948905683720000, -15.47720386886985544 ) ) ;
#3797 = EDGE_CURVE ( 'NONE', #19262, #5413, #5264, .T. ) ;
#3798 = CARTESIAN_POINT ( 'NONE',  ( -36.33955658999051508, 339.1198905601784759, 18.47759065022572500 ) ) ;
#3799 = EDGE_LOOP ( 'NONE', ( #15691, #8931, #10108, #9514 ) ) ;
#3800 = CARTESIAN_POINT ( 'NONE',  ( 20.42502041961814641, 160.1716627696692683, 40.00000000000000000 ) ) ;
#3801 = CARTESIAN_POINT ( 'NONE',  ( -40.01497788969913216, 338.8073905601784759, 16.95518130045146776 ) ) ;
#3802 = CARTESIAN_POINT ( 'NONE',  ( -11.93348319268871549, 308.8698905683720000, -2.051577885510841163E-15 ) ) ;
#3803 = EDGE_CURVE ( 'NONE', #19262, #1064, #20467, .T. ) ;
#3804 = CARTESIAN_POINT ( 'NONE',  ( -28.68588794268871567, 377.8698905683720000, 16.75240474999999307 ) ) ;
#3805 = CARTESIAN_POINT ( 'NONE',  ( -8.685887942688742314, 573.2448905601785327, 2.449293598294706119E-15 ) ) ;
#3806 = CARTESIAN_POINT ( 'NONE',  ( -28.68588794268873343, 524.4948905765655809, 19.99999999999999289 ) ) ;
#3807 = CARTESIAN_POINT ( 'NONE',  ( -42.88789093042844058, 412.9323905683720000, -9.489475012073736337 ) ) ;
#3808 = CARTESIAN_POINT ( 'NONE',  ( -35.09675569278793716, 257.2448905683720000, 15.47720386886985366 ) ) ;
#3809 = AXIS2_PLACEMENT_3D ( 'NONE', #17252, #13795, #18641 ) ;
#3810 = CARTESIAN_POINT ( 'NONE',  ( -45.43829269268871940, 423.8698905683720568, 0.000000000000000000 ) ) ;
#3811 = CONTEXT_DEPENDENT_SHAPE_REPRESENTATION ( #2265, #17872 ) ;
#3812 = CARTESIAN_POINT ( 'NONE',  ( -8.685887942688722774, 356.9948905765655809, -2.449293598294705724E-15 ) ) ;
#3813 = CARTESIAN_POINT ( 'NONE',  ( -8.685887942688722774, 362.2448905601784190, -2.449293598294705724E-15 ) ) ;
#3814 = CARTESIAN_POINT ( 'NONE',  ( -16.84014894278198327, 327.6198905683720000, 11.84573899990672530 ) ) ;
#3815 = CARTESIAN_POINT ( 'NONE',  ( -16.84014894278200103, 479.1198905683720000, 11.84573899990672530 ) ) ;
#3816 = EDGE_CURVE ( 'NONE', #6145, #10102, #18042, .T. ) ;
#3817 = CARTESIAN_POINT ( 'NONE',  ( -11.73070664223725501, 436.0573905765656377, 11.32908994701042005 ) ) ;
#3818 = LINE ( 'NONE', #7379, #18686 ) ;
#3819 = CARTESIAN_POINT ( 'NONE',  ( 0.5805565836007597902, 3.752776749732560368, -6.499999999999999112 ) ) ;
#3820 = VECTOR ( 'NONE', #14573, 1000.000000000000000 ) ;
#3821 = CARTESIAN_POINT ( 'NONE',  ( -40.53162694259543741, 384.1198905683720568, -11.84573899990672707 ) ) ;
#3822 = VECTOR ( 'NONE', #19254, 1000.000000000000000 ) ;
#3823 = CARTESIAN_POINT ( 'NONE',  ( -33.84809828339280102, 56.85652257517428865, -120.3299889578561448 ) ) ;
#3824 = AXIS2_PLACEMENT_3D ( 'NONE', #1218, #20896, #2942 ) ;
#3825 = CARTESIAN_POINT ( 'NONE',  ( -11.73070664223727100, 533.1823905601785327, -11.32908994701042715 ) ) ;
#3826 = CARTESIAN_POINT ( 'NONE',  ( -14.48388495494899786, 349.8073905683720000, -9.489475012073736337 ) ) ;
#3827 = EDGE_LOOP ( 'NONE', ( #6779, #19799, #12620, #19741 ) ) ;
#3828 = CARTESIAN_POINT ( 'NONE',  ( -32.01814843081346851, 521.6823905683720568, -16.75240474999999307 ) ) ;
#3829 = EDGE_LOOP ( 'NONE', ( #14865, #11737, #16377, #12568 ) ) ;
#3830 = DIRECTION ( 'NONE',  ( -0.8865057725575725689, 0.000000000000000000, 0.4627175328665443232 ) ) ;
#3831 = LINE ( 'NONE', #13687, #17400 ) ;
#3832 = EDGE_CURVE ( 'NONE', #12194, #17559, #1751, .T. ) ;
#3833 = LINE ( 'NONE', #7069, #2791 ) ;
#3834 = CARTESIAN_POINT ( 'NONE',  ( -10.20829729246300666, 527.6198905765656946, -7.653668647301794969 ) ) ;
#3835 = CARTESIAN_POINT ( 'NONE',  ( -44.16309181155857999, 474.4948905683720000, 6.410867750099241924 ) ) ;
#3836 = ORIENTED_EDGE ( 'NONE', *, *, #453, .F. ) ;
#3837 = CARTESIAN_POINT ( 'NONE',  ( -19.19641293061499709, 480.4323905683720568, -14.20200298773971603 ) ) ;
#3838 = CARTESIAN_POINT ( 'NONE',  ( -23.30663226349542327, 45.35645063453653592, -49.30906092905553351 ) ) ;
#3840 = VECTOR ( 'NONE', #2422, 999.9999999999998863 ) ;
#3839 = CARTESIAN_POINT ( 'NONE',  ( -42.82802356641966668, 423.2448905765656377, 14.14213562373094923 ) ) ;
#3841 = FACE_OUTER_BOUND ( 'NONE', #13554, .T. ) ;
#3842 = EDGE_CURVE ( 'NONE', #18961, #3882, #2727, .T. ) ;
#3843 = CARTESIAN_POINT ( 'NONE',  ( -8.685887942688715668, 302.2448905601784190, -2.449293598294705724E-15 ) ) ;
#3844 = CARTESIAN_POINT ( 'NONE',  ( -45.43829269268873361, 533.8698905683720568, 0.000000000000000000 ) ) ;
#3845 = CARTESIAN_POINT ( 'NONE',  ( -21.03221929538692336, 485.1198905765656377, 18.47759065022572500 ) ) ;
#3846 = CYLINDRICAL_SURFACE ( 'NONE', #16486, 19.99999999999999645 ) ;
#3847 = CARTESIAN_POINT ( 'NONE',  ( -36.33955658999051508, 435.3698905601784759, -18.47759065022572855 ) ) ;
#3848 = FACE_OUTER_BOUND ( 'NONE', #14624, .T. ) ;
#3849 = CARTESIAN_POINT ( 'NONE',  ( -28.68588794268870146, 277.8698905683720000, 16.75240474999999307 ) ) ;
#3850 = CARTESIAN_POINT ( 'NONE',  ( -8.685887942688724550, 366.9948905765655809, -2.449293598294705724E-15 ) ) ;
#3851 = CARTESIAN_POINT ( 'NONE',  ( -14.48388495494900852, 451.3073905683721136, -9.489475012073736337 ) ) ;
#3852 = CARTESIAN_POINT ( 'NONE',  ( -8.685887942688594876, 397.3073905765656946, -3.978247347592846594 ) ) ;
#3853 = CARTESIAN_POINT ( 'NONE',  ( -19.19641293061497578, 271.9323905683720568, -14.20200298773971603 ) ) ;
#3854 = ORIENTED_EDGE ( 'NONE', *, *, #8963, .T. ) ;
#3855 = CARTESIAN_POINT ( 'NONE',  ( -8.685887942688742314, 532.2448905601784190, -2.449293598294705724E-15 ) ) ;
#3856 = CARTESIAN_POINT ( 'NONE',  ( -28.68588794268872633, 477.8698905683720568, 16.75240474999999307 ) ) ;
#3857 = ADVANCED_FACE ( 'NONE', ( #1636, #20998 ), #6163, .F. ) ;
#3858 = ORIENTED_EDGE ( 'NONE', *, *, #14840, .F. ) ;
#3859 = CARTESIAN_POINT ( 'NONE',  ( -8.685887942688594876, 407.3073905765656946, -3.978247347592846594 ) ) ;
#3860 = CARTESIAN_POINT ( 'NONE',  ( -11.93348319268871016, 258.5573905683720568, 3.332260488124728415 ) ) ;
#3861 = ORIENTED_EDGE ( 'NONE', *, *, #13021, .T. ) ;
#3862 = DIRECTION ( 'NONE',  ( 1.000000000000000000, 0.000000000000000000, 0.000000000000000000 ) ) ;
#3863 = CARTESIAN_POINT ( 'NONE',  ( -11.93348319268871016, 270.3698905683720000, -2.051577885510841163E-15 ) ) ;
#3864 = CARTESIAN_POINT ( 'NONE',  ( -48.68588794268872277, 482.3073905765656377, 3.978247347593168115 ) ) ;
#3865 = CARTESIAN_POINT ( 'NONE',  ( -17.35679799567828852, 308.5573905765656946, -16.95518130045146421 ) ) ;
#3866 = CARTESIAN_POINT ( 'NONE',  ( -28.68588794268869790, 237.8698905683720568, 16.75240474999999307 ) ) ;
#3867 = CARTESIAN_POINT ( 'NONE',  ( -16.84014894278201169, 521.6198905683719431, -11.84573899990672707 ) ) ;
#3868 = CARTESIAN_POINT ( 'NONE',  ( -48.68588794268870856, 371.9948905765655809, 0.000000000000000000 ) ) ;
#3869 =( NAMED_UNIT ( * ) SI_UNIT ( $, .STERADIAN. ) SOLID_ANGLE_UNIT ( ) );
#3870 = CARTESIAN_POINT ( 'NONE',  ( -32.01814843081343298, 246.0573905683720000, 16.75240474999999307 ) ) ;
#3871 = AXIS2_PLACEMENT_3D ( 'NONE', #4595, #6316, #9561 ) ;
#3872 = CARTESIAN_POINT ( 'NONE',  ( -25.35362745456399125, 362.5573905683720568, -16.75240474999999307 ) ) ;
#3873 = EDGE_CURVE ( 'NONE', #1165, #13817, #11141, .T. ) ;
#3874 = CARTESIAN_POINT ( 'NONE',  ( -24.70764059509553690, 280.0573905601784759, 19.99999999999998934 ) ) ;
#3875 = CARTESIAN_POINT ( 'NONE',  ( -38.17536295476245556, 395.4323905683720000, 14.20200298773971781 ) ) ;
#3876 = CARTESIAN_POINT ( 'NONE',  ( -22.62331590640576451, 135.1716627696692683, -11.80838889663595914 ) ) ;
#3877 = CARTESIAN_POINT ( 'NONE',  ( -17.35679799567829562, 400.6823905601784759, 16.95518130045146421 ) ) ;
#3878 = EDGE_CURVE ( 'NONE', #16774, #17719, #16473, .T. ) ;
#3879 = VERTEX_POINT ( 'NONE', #14416 ) ;
#3880 = FACE_OUTER_BOUND ( 'NONE', #11169, .T. ) ;
#3881 = ORIENTED_EDGE ( 'NONE', *, *, #18949, .F. ) ;
#3882 = VERTEX_POINT ( 'NONE', #17746 ) ;
#3883 = CARTESIAN_POINT ( 'NONE',  ( -22.27502019258949417, 518.4948905683719431, 15.47720386886985189 ) ) ;
#3884 = CARTESIAN_POINT ( 'NONE',  ( -32.66413529028186957, 279.4323905601785327, 19.99999999999999289 ) ) ;
#3885 = CARTESIAN_POINT ( 'NONE',  ( -42.91714575264040121, 206.7622684196151965, -4.742258924317273916 ) ) ;
#3886 = ORIENTED_EDGE ( 'NONE', *, *, #20255, .F. ) ;
#3887 = CARTESIAN_POINT ( 'NONE',  ( -13.20868407381885667, 330.9948905683720000, -6.410867750099233042 ) ) ;
#3888 = CARTESIAN_POINT ( 'NONE',  ( -38.17536295476244845, 345.4323905683719431, 14.20200298773971781 ) ) ;
#3889 = CARTESIAN_POINT ( 'NONE',  ( -22.27502019258948707, 370.7448905683720568, -15.47720386886985544 ) ) ;
#3890 = CARTESIAN_POINT ( 'NONE',  ( -8.685887942688713892, 287.3073905765656377, -3.978247347593165895 ) ) ;
#3891 = DIRECTION ( 'NONE',  ( 0.000000000000000000, 0.000000000000000000, -1.000000000000000000 ) ) ;
#3892 = CARTESIAN_POINT ( 'NONE',  ( -45.43829269268870519, 273.8698905683720000, 0.000000000000000000 ) ) ;
#3893 = CARTESIAN_POINT ( 'NONE',  ( 0.000000000000000000, 610.7448905601785327, 0.000000000000000000 ) ) ;
#3894 = APPLICATION_CONTEXT ( 'automotive_design' ) ;
#3895 = AXIS2_PLACEMENT_3D ( 'NONE', #7348, #2718, #19045 ) ;
#3896 = CARTESIAN_POINT ( 'NONE',  ( -19.19641293061498999, 418.8073905683720568, 14.20200298773971426 ) ) ;
#3897 = CARTESIAN_POINT ( 'NONE',  ( -45.64106924314017988, 336.3073905601784759, -11.32908994701042538 ) ) ;
#3898 = CARTESIAN_POINT ( 'NONE',  ( -47.16347859291445843, 502.6198905765656377, 7.653668647301805628 ) ) ;
#3899 = DIRECTION ( 'NONE',  ( 0.000000000000000000, 1.000000000000000000, -0.000000000000000000 ) ) ;
#3900 = CARTESIAN_POINT ( 'NONE',  ( -35.09675569278794427, 327.2448905683720000, 15.47720386886985366 ) ) ;
#3901 = CARTESIAN_POINT ( 'NONE',  ( -19.19641293061499354, 460.4323905683721136, -14.20200298773971603 ) ) ;
#3902 = EDGE_LOOP ( 'NONE', ( #3568, #15957, #8962, #19985 ) ) ;
#3903 = CARTESIAN_POINT ( 'NONE',  ( -8.685887942688735208, 462.5573905601784759, -3.978247347593165895 ) ) ;
#3904 = CARTESIAN_POINT ( 'NONE',  ( -25.35362745456398414, 291.0573905683720000, -16.75240474999999307 ) ) ;
#3905 = AXIS2_PLACEMENT_3D ( 'NONE', #12646, #10898, #17614 ) ;
#3906 = EDGE_LOOP ( 'NONE', ( #14225, #475 ) ) ;
#3907 = ORIENTED_EDGE ( 'NONE', *, *, #7023, .T. ) ;
#3908 = CARTESIAN_POINT ( 'NONE',  ( -48.68588794268870146, 281.9948905765656377, 0.000000000000000000 ) ) ;
#3909 = CARTESIAN_POINT ( 'NONE',  ( -48.68588794268870856, 337.2448905601784759, 0.000000000000000000 ) ) ;
#3910 = AXIS2_PLACEMENT_3D ( 'NONE', #617, #7181, #722 ) ;
#3911 = CARTESIAN_POINT ( 'NONE',  ( -38.17536295476244845, 292.3073905683720000, -14.20200298773971426 ) ) ;
#3912 = CARTESIAN_POINT ( 'NONE',  ( -38.17536295476244845, 376.9323905683719431, 14.20200298773971781 ) ) ;
#3913 = CARTESIAN_POINT ( 'NONE',  ( -10.20829729246297646, 292.8698905601784759, -7.653668647301794969 ) ) ;
#3914 = CARTESIAN_POINT ( 'NONE',  ( -48.68588794268872988, 521.9948905765656946, 0.000000000000000000 ) ) ;
#3915 = CARTESIAN_POINT ( 'NONE',  ( -19.19641293061498999, 407.3073905683720000, 14.20200298773971426 ) ) ;
#3916 = CARTESIAN_POINT ( 'NONE',  ( -32.01814843081343298, 253.1823905683720568, -16.75240474999999307 ) ) ;
#3917 = CARTESIAN_POINT ( 'NONE',  ( -19.19641293061498999, 420.4323905683720000, -14.20200298773971603 ) ) ;
#3918 = CARTESIAN_POINT ( 'NONE',  ( -40.01497788969913927, 350.4323905765655809, -16.95518130045146421 ) ) ;
#3919 = FACE_OUTER_BOUND ( 'NONE', #20148, .T. ) ;
#3920 = CARTESIAN_POINT ( 'NONE',  ( -42.88789093042842637, 322.9323905683720568, -9.489475012073734561 ) ) ;
#3921 = CARTESIAN_POINT ( 'NONE',  ( -13.20868407381887266, 479.7448905683720568, 6.410867750099229490 ) ) ;
#3922 = EDGE_CURVE ( 'NONE', #14679, #13370, #6472, .T. ) ;
#3923 = VECTOR ( 'NONE', #7411, 1000.000000000000000 ) ;
#3924 = CARTESIAN_POINT ( 'NONE',  ( 44.98449999999999704, 0.000000000000000000, 0.000000000000000000 ) ) ;
#3925 = DIRECTION ( 'NONE',  ( 0.000000000000000000, 0.000000000000000000, -1.000000000000000000 ) ) ;
#3926 = CARTESIAN_POINT ( 'NONE',  ( 292.4526463419396691, 308.2087638784415162, 40.00000000000000000 ) ) ;
#3927 = EDGE_CURVE ( 'NONE', #20838, #9623, #1527, .T. ) ;
#3928 = CIRCLE ( 'NONE', #14314, 175.0000000000000284 ) ;
#3929 = EDGE_CURVE ( 'NONE', #5170, #5772, #14626, .T. ) ;
#3930 = CARTESIAN_POINT ( 'NONE',  ( -25.35362745456398414, 388.1823905683720568, 16.75240474999998952 ) ) ;
#3931 = CARTESIAN_POINT ( 'NONE',  ( -32.07601836630501424, 50.69989608122271818, -120.8146399612313502 ) ) ;
#3932 = CARTESIAN_POINT ( 'NONE',  ( -48.68588794268872988, 527.2448905601785327, 0.000000000000000000 ) ) ;
#3933 = CARTESIAN_POINT ( 'NONE',  ( -22.27502019258947641, 346.9948905683720000, 15.47720386886985189 ) ) ;
#3934 = ORIENTED_EDGE ( 'NONE', *, *, #19941, .F. ) ;
#3935 = CARTESIAN_POINT ( 'NONE',  ( -35.09675569278795848, 501.9948905683720000, -15.47720386886985544 ) ) ;
#3936 = ORIENTED_EDGE ( 'NONE', *, *, #11596, .F. ) ;
#3937 = CARTESIAN_POINT ( 'NONE',  ( -43.68588794268869435, 200.1437886375728965, 2.403080215999224424E-15 ) ) ;
#3938 = CARTESIAN_POINT ( 'NONE',  ( 40.42502041961814996, 180.1716627696692967, 40.00000000000000000 ) ) ;
#3939 = ADVANCED_FACE ( 'NONE', ( #3362, #13097, #11353 ), #17950, .T. ) ;
#3940 = CYLINDRICAL_SURFACE ( 'NONE', #17284, 220.7252770684332006 ) ;
#3941 = CARTESIAN_POINT ( 'NONE',  ( -11.73070664223726567, 493.1823905601785327, -11.32908994701042538 ) ) ;
#3942 = CARTESIAN_POINT ( 'NONE',  ( -35.09675569278795848, 471.9948905683720000, -15.47720386886985544 ) ) ;
#3943 = ORIENTED_EDGE ( 'NONE', *, *, #13996, .T. ) ;
#3944 = CARTESIAN_POINT ( 'NONE',  ( -16.84014894278200458, 480.1198905683720000, -11.84573899990672707 ) ) ;
#3945 = CARTESIAN_POINT ( 'NONE',  ( -8.685887942688884422, 251.9323905601784759, 3.978247347593586447 ) ) ;
#3946 = AXIS2_PLACEMENT_3D ( 'NONE', #5420, #2299, #12022 ) ;
#3947 = CARTESIAN_POINT ( 'NONE',  ( -28.68588794268872277, 409.4948905765656377, -19.99999999999999289 ) ) ;
#3948 = CARTESIAN_POINT ( 'NONE',  ( -17.35679799567830273, 475.4323905765655809, 16.95518130045146421 ) ) ;
#3949 = CARTESIAN_POINT ( 'NONE',  ( 20.42502041961814641, 160.1716627696692683, -61.32762281133329907 ) ) ;
#3950 = CARTESIAN_POINT ( 'NONE',  ( -24.70764059509557242, 484.4323905601785327, -19.99999999999999289 ) ) ;
#3951 = CARTESIAN_POINT ( 'NONE',  ( -11.73070664223726212, 486.0573905765656377, 11.32908994701042005 ) ) ;
#3952 = DIRECTION ( 'NONE',  ( -1.000000000000000000, -1.191790137725560488E-16, 0.000000000000000000 ) ) ;
#3953 = CARTESIAN_POINT ( 'NONE',  ( -14.54375231895777887, 433.4948905601784759, -14.14213562373094746 ) ) ;
#3954 = CARTESIAN_POINT ( 'NONE',  ( 0.000000000000000000, 5.629165124598848102, 3.250000000000005329 ) ) ;
#3955 = CARTESIAN_POINT ( 'NONE',  ( -45.43829269268869808, 275.0573905683720568, -3.332260488124726194 ) ) ;
#3956 = CARTESIAN_POINT ( 'NONE',  ( -21.03221929538690915, 254.1198905601784759, -18.47759065022572855 ) ) ;
#3957 = CARTESIAN_POINT ( 'NONE',  ( -45.64106924314017988, 362.9323905765656377, 11.32908994701042538 ) ) ;
#3958 = CARTESIAN_POINT ( 'NONE',  ( -11.93348319268873148, 450.0573905683719431, 3.332260488124728415 ) ) ;
#3959 = CARTESIAN_POINT ( 'NONE',  ( -47.16347859291444422, 331.3698905765656377, -7.653668647301793193 ) ) ;
#3960 = CARTESIAN_POINT ( 'NONE',  ( -38.17536295476244135, 276.9323905683720000, 14.20200298773971781 ) ) ;
#3961 = ORIENTED_EDGE ( 'NONE', *, *, #14142, .T. ) ;
#3962 = CARTESIAN_POINT ( 'NONE',  ( -45.43829269268872650, 485.0573905683721705, -3.332260488124726638 ) ) ;
#3963 = VERTEX_POINT ( 'NONE', #16562 ) ;
#3964 = DIRECTION ( 'NONE',  ( -1.000000000000000000, 0.000000000000000000, 0.000000000000000000 ) ) ;
#3965 = CARTESIAN_POINT ( 'NONE',  ( -45.43829269268869808, 243.8698905683720568, 0.000000000000000000 ) ) ;
#3966 = ORIENTED_EDGE ( 'NONE', *, *, #20990, .F. ) ;
#3967 = CARTESIAN_POINT ( 'NONE',  ( 166.1493775951145437, 620.7448905601785327, 8.917803138848105604 ) ) ;
#3968 = CARTESIAN_POINT ( 'NONE',  ( -40.01497788969914637, 483.5573905765655809, 16.95518130045146776 ) ) ;
#3969 = CARTESIAN_POINT ( 'NONE',  ( -54.57497958038185715, 230.5765313837437418, 25.00000000000000000 ) ) ;
#3970 = CARTESIAN_POINT ( 'NONE',  ( -38.86787825240671168, 223.9102039777116318, -13.30301237467029019 ) ) ;
#3971 = LINE ( 'NONE', #17395, #10841 ) ;
#3972 = CARTESIAN_POINT ( 'NONE',  ( -40.53162694259545873, 514.1198905683720568, -11.84573899990672707 ) ) ;
#3973 = LINE ( 'NONE', #20534, #20821 ) ;
#3974 = CARTESIAN_POINT ( 'NONE',  ( -45.43829269268869098, 253.5573905683720284, -3.332260488124726194 ) ) ;
#3975 = CARTESIAN_POINT ( 'NONE',  ( -14.48388495494899786, 341.3073905683720568, -9.489475012073736337 ) ) ;
#3976 = EDGE_CURVE ( 'NONE', #19193, #18799, #11998, .T. ) ;
#3977 = CARTESIAN_POINT ( 'NONE',  ( -48.68588794268870856, 351.9948905765656377, 0.000000000000000000 ) ) ;
#3978 = CARTESIAN_POINT ( 'NONE',  ( -28.68588794268871922, 401.3698905683720000, -16.75240474999999307 ) ) ;
#3979 = ADVANCED_FACE ( 'NONE', ( #10362 ), #18661, .T. ) ;
#3980 = CARTESIAN_POINT ( 'NONE',  ( 5.074999999999999289, 0.000000000000000000, 0.000000000000000000 ) ) ;
#3981 = CARTESIAN_POINT ( 'NONE',  ( -48.68588794268870856, 386.9323905601785327, -3.978247347593158345 ) ) ;
#3982 = ORIENTED_EDGE ( 'NONE', *, *, #15019, .F. ) ;
#3983 = ORIENTED_EDGE ( 'NONE', *, *, #17042, .T. ) ;
#3984 = VERTEX_POINT ( 'NONE', #14928 ) ;
#3985 = CARTESIAN_POINT ( 'NONE',  ( -32.01814843081346851, 507.5573905683720568, 16.75240474999999307 ) ) ;
#3986 = CARTESIAN_POINT ( 'NONE',  ( -8.685887942688539809, 317.3073905765655809, -3.978247347592740013 ) ) ;
#3987 = ORIENTED_EDGE ( 'NONE', *, *, #13718, .F. ) ;
#3988 = CARTESIAN_POINT ( 'NONE',  ( -35.09675569278793716, 303.4948905683720568, -15.47720386886985544 ) ) ;
#3989 = VERTEX_POINT ( 'NONE', #110 ) ;
#3990 = CARTESIAN_POINT ( 'NONE',  ( -19.19641293061498288, 340.4323905683720000, -14.20200298773971603 ) ) ;
#3991 = CARTESIAN_POINT ( 'NONE',  ( -22.27502019258948707, 350.7448905683720568, -15.47720386886985544 ) ) ;
#3992 = CARTESIAN_POINT ( 'NONE',  ( -24.70764059509555466, 289.1823905765656377, -19.99999999999999289 ) ) ;
#3993 = CARTESIAN_POINT ( 'NONE',  ( -8.685887942688738761, 496.9948905765655809, -2.449293598294705724E-15 ) ) ;
#3994 = CARTESIAN_POINT ( 'NONE',  ( -44.16309181155855157, 244.4948905683720284, 6.410867750099241924 ) ) ;
#3995 = CARTESIAN_POINT ( 'NONE',  ( -42.82802356641964536, 225.9948905601784759, -14.14213562373094746 ) ) ;
#3996 = CARTESIAN_POINT ( 'NONE',  ( -45.43829269268871229, 395.6823905683719431, 3.332260488124734632 ) ) ;
#3997 = ADVANCED_FACE ( 'NONE', ( #20107 ), #5276, .F. ) ;
#3998 = CARTESIAN_POINT ( 'NONE',  ( -17.35679799567829207, 333.8073905601784759, -16.95518130045146421 ) ) ;
#3999 = CARTESIAN_POINT ( 'NONE',  ( -17.35679799567830628, 448.5573905765656946, -16.95518130045146421 ) ) ;
#4000 = UNCERTAINTY_MEASURE_WITH_UNIT (LENGTH_MEASURE( 1.000000000000000082E-05 ), #7374, 'distance_accuracy_value', 'NONE');
#4001 = CARTESIAN_POINT ( 'NONE',  ( -31.26501780185373391, 205.1437886375728965, -5.000000000000001776 ) ) ;
#4002 = CARTESIAN_POINT ( 'NONE',  ( -42.88789093042842637, 314.4323905683720000, -9.489475012073736337 ) ) ;
#4003 = CARTESIAN_POINT ( 'NONE',  ( -45.43829269268871940, 454.1823905683720568, 3.332260488124734632 ) ) ;
#4004 = ORIENTED_EDGE ( 'NONE', *, *, #10480, .F. ) ;
#4005 = CARTESIAN_POINT ( 'NONE',  ( -36.33955658999052218, 475.3698905601784759, -18.47759065022572855 ) ) ;
#4006 = CARTESIAN_POINT ( 'NONE',  ( -28.68588794268870146, 286.3698905683720568, 16.75240474999999307 ) ) ;
#4007 = ORIENTED_EDGE ( 'NONE', *, *, #20720, .T. ) ;
#4008 = CARTESIAN_POINT ( 'NONE',  ( -40.01497788969913216, 338.8073905601784190, 16.95518130045146776 ) ) ;
#4009 = ORIENTED_EDGE ( 'NONE', *, *, #2400, .F. ) ;
#4010 = ORIENTED_EDGE ( 'NONE', *, *, #6564, .T. ) ;
#4011 = LINE ( 'NONE', #4119, #5950 ) ;
#4012 = CARTESIAN_POINT ( 'NONE',  ( -47.16347859291444422, 347.8698905601784759, 7.653668647301805628 ) ) ;
#4013 = CARTESIAN_POINT ( 'NONE',  ( -16.84014894278198327, 310.1198905683720000, -11.84573899990672707 ) ) ;
#4014 = ADVANCED_FACE ( 'NONE', ( #2050 ), #8624, .T. ) ;
#4015 = CARTESIAN_POINT ( 'NONE',  ( -40.53162694259543741, 386.6198905683720568, 11.84573899990672885 ) ) ;
#4016 = AXIS2_PLACEMENT_3D ( 'NONE', #9698, #21174, #10998 ) ;
#4017 = CARTESIAN_POINT ( 'NONE',  ( -28.68588794268870856, 294.7448905601784759, -19.99999999999999289 ) ) ;
#4018 = CARTESIAN_POINT ( 'NONE',  ( -21.03221929538694468, 528.8698905765656946, -18.47759065022572855 ) ) ;
#4019 = CARTESIAN_POINT ( 'NONE',  ( -11.93348319268872615, 408.8698905683720568, -2.051577885510841163E-15 ) ) ;
#4020 = CARTESIAN_POINT ( 'NONE',  ( -44.16309181155855867, 244.7448905683720000, -6.410867750099231266 ) ) ;
#4021 = CARTESIAN_POINT ( 'NONE',  ( -40.53162694259544452, 402.6198905683720568, -11.84573899990672707 ) ) ;
#4022 = ITEM_DEFINED_TRANSFORMATION ( 'NONE', 'NONE', #2813,  #12794 ) ;
#4023 = CIRCLE ( 'NONE', #1615, 9.999999999999994671 ) ;
#4024 = CARTESIAN_POINT ( 'NONE',  ( -48.68588794268870856, 341.9948905765656377, 0.000000000000000000 ) ) ;
#4025 = DIRECTION ( 'NONE',  ( -0.000000000000000000, 1.000000000000000000, -0.000000000000000000 ) ) ;
#4026 = CARTESIAN_POINT ( 'NONE',  ( -45.43829269268870519, 313.8698905683720000, 0.000000000000000000 ) ) ;
#4027 =( LENGTH_UNIT ( ) NAMED_UNIT ( * ) SI_UNIT ( .MILLI., .METRE. ) );
#4028 = CARTESIAN_POINT ( 'NONE',  ( -45.43829269268871940, 475.6823905683720000, 3.332260488124734632 ) ) ;
#4029 = ADVANCED_FACE ( 'NONE', ( #20212 ), #2153, .F. ) ;
#4030 = CARTESIAN_POINT ( 'NONE',  ( -10.20829729246299422, 436.3698905765656377, 7.653668647301790529 ) ) ;
#4031 = CARTESIAN_POINT ( 'NONE',  ( -22.62331590640576096, 213.9102039777116602, 11.80838889663596447 ) ) ;
#4032 = CARTESIAN_POINT ( 'NONE',  ( 30.42502041961813575, 271.1055109169419097, 40.00000000000000000 ) ) ;
#4033 = AXIS2_PLACEMENT_3D ( 'NONE', #5160, #13499, #3539 ) ;
#4034 = CARTESIAN_POINT ( 'NONE',  ( -25.35362745456399480, 392.5573905683720000, -16.75240474999999307 ) ) ;
#4035 = LINE ( 'NONE', #17033, #17849 ) ;
#4036 = CARTESIAN_POINT ( 'NONE',  ( -14.54375231895779130, 533.4948905601785327, -14.14213562373094746 ) ) ;
#4037 = CARTESIAN_POINT ( 'NONE',  ( -19.19641293061497933, 337.3073905683720568, 14.20200298773971426 ) ) ;
#4038 = VECTOR ( 'NONE', #11393, 1000.000000000000000 ) ;
#4039 = ORIENTED_EDGE ( 'NONE', *, *, #8948, .T. ) ;
#4040 = CARTESIAN_POINT ( 'NONE',  ( -16.84014894278200813, 510.1198905683720568, -11.84573899990672707 ) ) ;
#4041 = ORIENTED_EDGE ( 'NONE', *, *, #13300, .T. ) ;
#4042 = ADVANCED_BREP_SHAPE_REPRESENTATION ( '', ( #4359, #12794 ), #20056 ) ;
#4043 = FACE_OUTER_BOUND ( 'NONE', #8124, .T. ) ;
#4044 = LINE ( 'NONE', #1033, #2206 ) ;
#4045 = DIRECTION ( 'NONE',  ( 0.000000000000000000, 0.8660254037844375974, -0.5000000000000019984 ) ) ;
#4046 = LINE ( 'NONE', #12493, #3471 ) ;
#4047 = CARTESIAN_POINT ( 'NONE',  ( -35.09675569278796559, 455.7448905683720568, 15.47720386886985366 ) ) ;
#4048 = EDGE_LOOP ( 'NONE', ( #6699, #11120, #20618, #13525 ) ) ;
#4049 = CARTESIAN_POINT ( 'NONE',  ( -16.84014894278200103, 477.6198905683720000, 11.84573899990672530 ) ) ;
#4050 = CARTESIAN_POINT ( 'NONE',  ( -17.35679799567827786, 245.4323905765656377, 16.95518130045146421 ) ) ;
#4051 = CIRCLE ( 'NONE', #20287, 175.0000000000000284 ) ;
#4052 = CARTESIAN_POINT ( 'NONE',  ( -21.03221929538691626, 405.1198905765656377, 18.47759065022572500 ) ) ;
#4053 = CARTESIAN_POINT ( 'NONE',  ( -40.01497788969914637, 473.5573905765655809, 16.95518130045146776 ) ) ;
#4054 = CARTESIAN_POINT ( 'NONE',  ( 45.67500000000000426, 0.000000000000000000, 0.000000000000000000 ) ) ;
#4055 = CARTESIAN_POINT ( 'NONE',  ( -8.685887942688719221, 332.2448905601784759, -2.449293598294705724E-15 ) ) ;
#4056 = CARTESIAN_POINT ( 'NONE',  ( 43.53705524234220547, 56.85652257517428865, 96.62835994548002816 ) ) ;
#4057 = AXIS2_PLACEMENT_3D ( 'NONE', #7901, #12901, #17860 ) ;
#4058 = CARTESIAN_POINT ( 'NONE',  ( -28.68588794268870501, 259.4948905765655809, -19.99999999999999289 ) ) ;
#4059 = CARTESIAN_POINT ( 'NONE',  ( -28.68588794268869790, 239.7448905601785043, 19.99999999999999289 ) ) ;
#4060 = PLANE ( 'NONE',  #15942 ) ;
#4061 = EDGE_CURVE ( 'NONE', #12399, #2614, #14247, .T. ) ;
#4062 = CARTESIAN_POINT ( 'NONE',  ( -42.88789093042842637, 274.4323905683720568, -9.489475012073736337 ) ) ;
#4063 = EDGE_CURVE ( 'NONE', #4339, #6752, #1075, .T. ) ;
#4064 = CARTESIAN_POINT ( 'NONE',  ( -8.685887942688708563, 251.9323905601784475, 3.978247347593161010 ) ) ;
#4065 = CARTESIAN_POINT ( 'NONE',  ( -36.33955658999052218, 403.8698905765656377, 18.47759065022572500 ) ) ;
#4066 = CARTESIAN_POINT ( 'NONE',  ( -22.27502019258949773, 452.2448905683720000, -15.47720386886985544 ) ) ;
#4067 = CARTESIAN_POINT ( 'NONE',  ( -11.73070664223724613, 327.9323905765656377, -11.32908994701042538 ) ) ;
#4068 = CARTESIAN_POINT ( 'NONE',  ( -32.01814843081343298, 273.1823905683720568, -16.75240474999999307 ) ) ;
#4069 = ORIENTED_EDGE ( 'NONE', *, *, #15846, .T. ) ;
#4070 = ORIENTED_EDGE ( 'NONE', *, *, #13331, .T. ) ;
#4071 = CARTESIAN_POINT ( 'NONE',  ( -22.27502019258949773, 482.2448905683720568, -15.47720386886985544 ) ) ;
#4072 = ORIENTED_EDGE ( 'NONE', *, *, #4537, .F. ) ;
#4073 = DIRECTION ( 'NONE',  ( -1.191790137725560488E-16, 1.000000000000000000, -0.000000000000000000 ) ) ;
#4074 = CARTESIAN_POINT ( 'NONE',  ( -45.43829269268869098, 244.1823905683720568, 3.332260488124734632 ) ) ;
#4075 = ORIENTED_EDGE ( 'NONE', *, *, #17946, .T. ) ;
#4076 = SHAPE_REPRESENTATION ( 'hex screw gradeab_iso_ISO 4017 - M8 x 16-N', ( #12794 ), #12451 ) ;
#4077 = CARTESIAN_POINT ( 'NONE',  ( -8.685887942688717445, 306.9948905765655809, -2.449293598294705724E-15 ) ) ;
#4078 = CARTESIAN_POINT ( 'NONE',  ( -47.16347859291445843, 461.3698905765656377, -7.653668647301793193 ) ) ;
#4079 = CARTESIAN_POINT ( 'NONE',  ( -47.16347859291444422, 387.8698905601784759, 7.653668647301805628 ) ) ;
#4080 = CARTESIAN_POINT ( 'NONE',  ( -32.66413529028188378, 455.0573905601785896, -19.99999999999999289 ) ) ;
#4081 = CARTESIAN_POINT ( 'NONE',  ( -35.09675569278793006, 233.4948905683720284, -15.47720386886985544 ) ) ;
#4082 = CARTESIAN_POINT ( 'NONE',  ( -32.01814843081346851, 513.1823905683720568, -16.75240474999999307 ) ) ;
#4083 = DIRECTION ( 'NONE',  ( 1.000000000000000000, -0.000000000000000000, -0.000000000000000000 ) ) ;
#4084 = CARTESIAN_POINT ( 'NONE',  ( -45.43829269268869808, 253.8698905683720000, 0.000000000000000000 ) ) ;
#4085 = CARTESIAN_POINT ( 'NONE',  ( -14.48388495494899608, 339.4323905683720000, 9.489475012073732785 ) ) ;
#4086 = CARTESIAN_POINT ( 'NONE',  ( -40.01497788969912506, 318.8073905601784759, 16.95518130045146776 ) ) ;
#4087 = CARTESIAN_POINT ( 'NONE',  ( -32.66413529028186957, 359.4323905601785327, 19.99999999999999289 ) ) ;
#4088 = CARTESIAN_POINT ( 'NONE',  ( -16.84014894278199392, 380.1198905683720568, -11.84573899990672707 ) ) ;
#4089 = CARTESIAN_POINT ( 'NONE',  ( 10.41669750159067220, 217.7548513357008630, 45.00000000000000000 ) ) ;
#4090 = CARTESIAN_POINT ( 'NONE',  ( -11.73070664223725323, 393.1823905601785896, -11.32908994701042715 ) ) ;
#4091 = AXIS2_PLACEMENT_3D ( 'NONE', #14778, #11299, #1364 ) ;
#4092 = DIRECTION ( 'NONE',  ( -1.191790137725560488E-16, 1.000000000000000000, -0.000000000000000000 ) ) ;
#4093 = ORIENTED_EDGE ( 'NONE', *, *, #1422, .T. ) ;
#4094 = ORIENTED_EDGE ( 'NONE', *, *, #16856, .T. ) ;
#4095 = CARTESIAN_POINT ( 'NONE',  ( -11.93348319268873858, 510.0573905683720000, 3.332260488124728415 ) ) ;
#4096 = CARTESIAN_POINT ( 'NONE',  ( -54.57497958038185715, 303.6587712403113528, 25.00000000000000000 ) ) ;
#4097 = ORIENTED_EDGE ( 'NONE', *, *, #8549, .T. ) ;
#4098 = CARTESIAN_POINT ( 'NONE',  ( -11.93348319268871549, 310.3698905683720568, -2.051577885510841163E-15 ) ) ;
#4099 = VERTEX_POINT ( 'NONE', #5809 ) ;
#4100 = CARTESIAN_POINT ( 'NONE',  ( -14.48388495494899608, 337.9323905683720568, 9.489475012073732785 ) ) ;
#4101 = CARTESIAN_POINT ( 'NONE',  ( -38.17536295476244845, 355.4323905683720568, 14.20200298773971781 ) ) ;
#4102 = CARTESIAN_POINT ( 'NONE',  ( -17.35679799567829207, 288.5573905765656377, -16.95518130045146421 ) ) ;
#4103 = CARTESIAN_POINT ( 'NONE',  ( -17.35679799567831338, 498.5573905765655809, -16.95518130045146421 ) ) ;
#4104 = CARTESIAN_POINT ( 'NONE',  ( -35.09675569278793716, 245.7448905683720000, 15.47720386886985366 ) ) ;
#4105 = CARTESIAN_POINT ( 'NONE',  ( -43.63022347157594538, 200.3131325479159273, 1.300740588846954759 ) ) ;
#4106 = CARTESIAN_POINT ( 'NONE',  ( -42.88789093042844058, 404.4323905683721136, -9.489475012073736337 ) ) ;
#4107 = CIRCLE ( 'NONE', #16215, 4.999999999999990230 ) ;
#4108 = LINE ( 'NONE', #997, #16502 ) ;
#4109 = CARTESIAN_POINT ( 'NONE',  ( -28.68588794268872988, 504.4948905765655809, 19.99999999999999289 ) ) ;
#4110 = CARTESIAN_POINT ( 'NONE',  ( -32.66413529028185536, 245.0573905601785043, -19.99999999999999289 ) ) ;
#4111 = CARTESIAN_POINT ( 'NONE',  ( -32.01814843081346140, 461.6823905683720568, -16.75240474999999307 ) ) ;
#4112 = CIRCLE ( 'NONE', #17930, 20.57735571454641033 ) ;
#4113 = ORIENTED_EDGE ( 'NONE', *, *, #7561, .T. ) ;
#4114 = CARTESIAN_POINT ( 'NONE',  ( -17.35679799567830273, 450.6823905601785327, 16.95518130045146421 ) ) ;
#4115 = ORIENTED_EDGE ( 'NONE', *, *, #14849, .T. ) ;
#4116 = LINE ( 'NONE', #7460, #8398 ) ;
#4117 = EDGE_LOOP ( 'NONE', ( #20440, #7732, #16535, #16217, #12982, #14390, #5983, #6989, #3907, #9336, #3543, #2276, #8119, #9726, #17201 ) ) ;
#4118 = ORIENTED_EDGE ( 'NONE', *, *, #7307, .T. ) ;
#4119 = CARTESIAN_POINT ( 'NONE',  ( 45.67500000000000426, 0.000000000000000000, 3.309499999999999886 ) ) ;
#4120 = CARTESIAN_POINT ( 'NONE',  ( -28.68588794268871212, 334.7448905601784759, -19.99999999999999289 ) ) ;
#4121 = CARTESIAN_POINT ( 'NONE',  ( -14.48388495494899075, 307.9323905683720000, 9.489475012073732785 ) ) ;
#4122 = AXIS2_PLACEMENT_3D ( 'NONE', #7025, #11901, #11795 ) ;
#4123 = EDGE_CURVE ( 'NONE', #13817, #7658, #10458, .T. ) ;
#4124 = CARTESIAN_POINT ( 'NONE',  ( -32.01814843081344719, 357.5573905683720000, 16.75240474999999307 ) ) ;
#4125 = CARTESIAN_POINT ( 'NONE',  ( -21.03221929538691626, 294.1198905601785327, -18.47759065022572855 ) ) ;
#4126 = CARTESIAN_POINT ( 'NONE',  ( -45.64106924314020119, 531.0573905765656946, -11.32908994701042715 ) ) ;
#4127 = CARTESIAN_POINT ( 'NONE',  ( -40.53162694259544452, 405.1198905683720000, 11.84573899990672885 ) ) ;
#4128 = CARTESIAN_POINT ( 'NONE',  ( -19.19641293061497223, 231.9323905683720000, -14.20200298773971603 ) ) ;
#4129 = CARTESIAN_POINT ( 'NONE',  ( -38.17536295476246266, 412.3073905683720000, -14.20200298773971426 ) ) ;
#4130 = CARTESIAN_POINT ( 'NONE',  ( -47.16347859291444422, 352.6198905765656377, 7.653668647301805628 ) ) ;
#4131 = CARTESIAN_POINT ( 'NONE',  ( -28.68588794268874054, 608.2448905601786464, 20.00000000000000000 ) ) ;
#4132 = CARTESIAN_POINT ( 'NONE',  ( -28.68588794268870856, 311.3698905683720568, -16.75240474999999307 ) ) ;
#4133 = CARTESIAN_POINT ( 'NONE',  ( -32.01814843081346140, 463.1823905683720000, -16.75240474999999307 ) ) ;
#4134 = CARTESIAN_POINT ( 'NONE',  ( -32.66413529028189089, 514.1823905765656946, 19.99999999999999289 ) ) ;
#4135 = DIRECTION ( 'NONE',  ( 0.9999562017632421806, 0.000000000000000000, -0.009359196291876339252 ) ) ;
#4136 = CARTESIAN_POINT ( 'NONE',  ( 52.60622592008805043, 30.52886280891152282, 151.0302712373927250 ) ) ;
#4137 = EDGE_CURVE ( 'NONE', #6325, #21365, #20888, .T. ) ;
#4138 = CARTESIAN_POINT ( 'NONE',  ( -25.35362745456398059, 368.1823905683721136, 16.75240474999998952 ) ) ;
#4139 = DIRECTION ( 'NONE',  ( 1.232945044042657126E-32, -9.855701800883825964E-17, 1.000000000000000000 ) ) ;
#4140 = CARTESIAN_POINT ( 'NONE',  ( -32.66413529028189799, 509.4323905601784190, 19.99999999999999289 ) ) ;
#4141 = CARTESIAN_POINT ( 'NONE',  ( -45.43829269268871229, 333.8698905683720000, 0.000000000000000000 ) ) ;
#4142 = ORIENTED_EDGE ( 'NONE', *, *, #16439, .F. ) ;
#4143 = CARTESIAN_POINT ( 'NONE',  ( -42.88789093042845479, 512.9323905683719431, -9.489475012073736337 ) ) ;
#4144 = ORIENTED_EDGE ( 'NONE', *, *, #13811, .T. ) ;
#4145 = CARTESIAN_POINT ( 'NONE',  ( -11.73070664223724613, 351.3073905601785327, 11.32908994701042005 ) ) ;
#4146 = EDGE_CURVE ( 'NONE', #17095, #3367, #6026, .T. ) ;
#4147 = DIRECTION ( 'NONE',  ( 0.000000000000000000, -0.000000000000000000, 1.000000000000000000 ) ) ;
#4148 = EDGE_CURVE ( 'NONE', #20120, #6145, #3973, .T. ) ;
#4149 = CARTESIAN_POINT ( 'NONE',  ( -16.84014894278199748, 421.6198905683720000, -11.84573899990672707 ) ) ;
#4150 = CARTESIAN_POINT ( 'NONE',  ( 20.42502041961813575, 271.1055109169419666, -40.00000000000000000 ) ) ;
#4151 = CARTESIAN_POINT ( 'NONE',  ( -28.68588794268874054, 573.2448905601785327, 0.000000000000000000 ) ) ;
#4152 = CARTESIAN_POINT ( 'NONE',  ( -13.20868407381887444, 469.4948905683720000, -6.410867750099233042 ) ) ;
#4153 = ORIENTED_EDGE ( 'NONE', *, *, #20293, .F. ) ;
#4154 = CARTESIAN_POINT ( 'NONE',  ( -42.88789093042844769, 462.9323905683720568, -9.489475012073734561 ) ) ;
#4155 = LINE ( 'NONE', #5774, #344 ) ;
#4156 = CARTESIAN_POINT ( 'NONE',  ( -10.20829729246299067, 396.3698905765656377, 7.653668647301790529 ) ) ;
#4157 = DIRECTION ( 'NONE',  ( -1.191790137725560488E-16, 1.000000000000000000, -0.000000000000000000 ) ) ;
#4158 = CARTESIAN_POINT ( 'NONE',  ( -45.64106924314017277, 298.1823905601785327, 11.32908994701042538 ) ) ;
#4159 = CARTESIAN_POINT ( 'NONE',  ( 0.1061556211655317883, 4.836380039389415408, -4.623144047065555817 ) ) ;
#4160 = DIRECTION ( 'NONE',  ( -0.000000000000000000, -1.000000000000000000, 0.000000000000000000 ) ) ;
#4161 = VECTOR ( 'NONE', #8613, 1000.000000000000000 ) ;
#4162 = DIRECTION ( 'NONE',  ( -0.000000000000000000, -0.000000000000000000, 1.000000000000000000 ) ) ;
#4163 = SURFACE_STYLE_FILL_AREA ( #9133 ) ;
#4164 = CARTESIAN_POINT ( 'NONE',  ( 0.5805565836007611225, -3.752776749732563033, 6.500000000000000000 ) ) ;
#4165 = CIRCLE ( 'NONE', #6920, 3.309499999999999886 ) ;
#4166 = CARTESIAN_POINT ( 'NONE',  ( -40.53162694259543031, 274.1198905683720568, -11.84573899990672707 ) ) ;
#4167 = CARTESIAN_POINT ( 'NONE',  ( -36.33955658999049376, 245.3698905601785043, -18.47759065022572855 ) ) ;
#4168 = CARTESIAN_POINT ( 'NONE',  ( -45.64106924314018698, 402.9323905765656946, 11.32908994701042538 ) ) ;
#4169 = CARTESIAN_POINT ( 'NONE',  ( -28.68588794268871922, 417.8698905683720568, 16.75240474999999307 ) ) ;
#4170 = CARTESIAN_POINT ( 'NONE',  ( -42.82802356641966668, 400.7448905765656377, -14.14213562373094746 ) ) ;
#4171 = VECTOR ( 'NONE', #15562, 1000.000000000000000 ) ;
#4172 = CARTESIAN_POINT ( 'NONE',  ( -28.68588794268870501, 262.8698905683720000, -16.75240474999999307 ) ) ;
#4173 = B_SPLINE_CURVE_WITH_KNOTS ( 'NONE', 3,
 ( #17861, #6287, #2849, #16259, #1438, #8007, #9215, #15836 ),
 .UNSPECIFIED., .F., .F.,
 ( 4, 2, 2, 4 ),
 ( 0.003797433802554436334, 0.004743183970586235289, 0.005688934138618035111, 0.007580434474681631285 ),
 .UNSPECIFIED. ) ;
#4174 = ORIENTED_EDGE ( 'NONE', *, *, #3353, .T. ) ;
#4175 = AXIS2_PLACEMENT_3D ( 'NONE', #7920, #7818, #6199 ) ;
#4176 = DIRECTION ( 'NONE',  ( -0.000000000000000000, -1.000000000000000000, -0.000000000000000000 ) ) ;
#4177 = EDGE_LOOP ( 'NONE', ( #3308, #13446, #6905, #1212 ) ) ;
#4178 = CARTESIAN_POINT ( 'NONE',  ( -44.16309181155858710, 474.7448905683720568, -6.410867750099231266 ) ) ;
#4179 = VECTOR ( 'NONE', #6208, 1000.000000000000114 ) ;
#4180 = VECTOR ( 'NONE', #17889, 1000.000000000000000 ) ;
#4181 = VERTEX_POINT ( 'NONE', #7646 ) ;
#4182 = CARTESIAN_POINT ( 'NONE',  ( -32.66413529028189089, 524.1823905765656946, 19.99999999999999289 ) ) ;
#4183 = CARTESIAN_POINT ( 'NONE',  ( -16.84014894278197261, 237.6198905683720284, 11.84573899990672530 ) ) ;
#4184 = APPLICATION_CONTEXT ( 'automotive_design' ) ;
#4185 = EDGE_LOOP ( 'NONE', ( #8234, #2377, #20435, #7883 ) ) ;
#4186 = CARTESIAN_POINT ( 'NONE',  ( -11.93348319268874214, 528.5573905683720568, 3.332260488124728859 ) ) ;
#4187 = CARTESIAN_POINT ( 'NONE',  ( 5.674999999999999822, 7.505553499465139389, 0.000000000000000000 ) ) ;
#4188 = CARTESIAN_POINT ( 'NONE',  ( -17.35679799567830983, 468.5573905765655809, -16.95518130045146421 ) ) ;
#4189 = CARTESIAN_POINT ( 'NONE',  ( 20.42502041961813930, 230.5765313837437418, 49.99999999999999289 ) ) ;
#4190 = SURFACE_STYLE_USAGE ( .BOTH. , #20631 ) ;
#4191 = CARTESIAN_POINT ( 'NONE',  ( 78.68120802659203150, 149.7457237375499517, 66.14548919766383506 ) ) ;
#4192 = DIRECTION ( 'NONE',  ( -0.000000000000000000, 1.000000000000000000, -0.000000000000000000 ) ) ;
#4193 = CARTESIAN_POINT ( 'NONE',  ( -11.93348319268873858, 510.3698905683720000, -2.051577885510841163E-15 ) ) ;
#4194 = DIRECTION ( 'NONE',  ( 0.000000000000000000, 0.000000000000000000, 1.000000000000000000 ) ) ;
#4195 = CARTESIAN_POINT ( 'NONE',  ( -11.93348319268870839, 238.5573905683720000, 3.332260488124728415 ) ) ;
#4196 = CARTESIAN_POINT ( 'NONE',  ( -28.68588794268870856, 337.8698905683720000, 16.75240474999999307 ) ) ;
#4197 = EDGE_CURVE ( 'NONE', #5663, #6477, #7425, .T. ) ;
#4198 = CARTESIAN_POINT ( 'NONE',  ( -11.73070664223725856, 471.3073905601784759, 11.32908994701042005 ) ) ;
#4199 = CARTESIAN_POINT ( 'NONE',  ( -8.685887942688985675, 361.9323905601784759, 3.978247347593800054 ) ) ;
#4200 = AXIS2_PLACEMENT_3D ( 'NONE', #4096, #5933, #2704 ) ;
#4201 = EDGE_CURVE ( 'NONE', #11949, #6011, #20636, .T. ) ;
#4202 = ADVANCED_FACE ( 'NONE', ( #2366 ), #17496, .F. ) ;
#4203 = CARTESIAN_POINT ( 'NONE',  ( -35.09675569278795138, 391.9948905683720568, -15.47720386886985544 ) ) ;
#4204 = UNCERTAINTY_MEASURE_WITH_UNIT (LENGTH_MEASURE( 1.000000000000000082E-05 ), #10723, 'distance_accuracy_value', 'NONE');
#4205 = CARTESIAN_POINT ( 'NONE',  ( -14.54375231895776288, 325.7448905765655809, 14.14213562373094568 ) ) ;
#4206 = SHAPE_REPRESENTATION ( 'Coarse Pitch Steep Screw Shaft', ( #12794 ), #4502 ) ;
#4207 = CARTESIAN_POINT ( 'NONE',  ( -28.68588794268871922, 394.7448905601784759, -19.99999999999999289 ) ) ;
#4208 = VERTEX_POINT ( 'NONE', #10780 ) ;
#4209 = CARTESIAN_POINT ( 'NONE',  ( 2.085632741019731137E-15, 575.7448905601785327, 0.000000000000000000 ) ) ;
#4210 = ORIENTED_EDGE ( 'NONE', *, *, #1780, .F. ) ;
#4211 = VERTEX_POINT ( 'NONE', #2686 ) ;
#4212 = CARTESIAN_POINT ( 'NONE',  ( -14.48388495494901740, 501.3073905683720568, -9.489475012073736337 ) ) ;
#4213 = CARTESIAN_POINT ( 'NONE',  ( -32.66413529028186247, 294.1823905765655809, 19.99999999999999289 ) ) ;
#4214 = ORIENTED_EDGE ( 'NONE', *, *, #12793, .T. ) ;
#4215 = EDGE_CURVE ( 'NONE', #880, #4398, #2580, .T. ) ;
#4216 = CARTESIAN_POINT ( 'NONE',  ( -35.09675569278793716, 313.4948905683720000, -15.47720386886985544 ) ) ;
#4217 = VERTEX_POINT ( 'NONE', #9271 ) ;
#4218 = CARTESIAN_POINT ( 'NONE',  ( -38.17536295476245556, 342.3073905683721136, -14.20200298773971426 ) ) ;
#4219=STYLED_ITEM('',(#21449),#4359);
#4220 = CARTESIAN_POINT ( 'NONE',  ( -22.27502019258948351, 340.7448905683720568, -15.47720386886985544 ) ) ;
#4221 = CARTESIAN_POINT ( 'NONE',  ( -14.54375231895775578, 275.7448905765656377, 14.14213562373094568 ) ) ;
#4222 = CARTESIAN_POINT ( 'NONE',  ( -8.685887942688742314, 573.2448905601785327, 2.449293598294706119E-15 ) ) ;
#4223 = CARTESIAN_POINT ( 'NONE',  ( -13.20868407381884779, 249.4948905683720284, -6.410867750099233042 ) ) ;
#4224 = CARTESIAN_POINT ( 'NONE',  ( 5.074999999999999289, -3.752776749732576356, -6.500000000000000000 ) ) ;
#4225 = MANIFOLD_SOLID_BREP ( 'Boss-Extrude22', #11056 ) ;
#4226 = CARTESIAN_POINT ( 'NONE',  ( -28.68588794268871567, 397.8698905683720000, 16.75240474999999307 ) ) ;
#4227 = CARTESIAN_POINT ( 'NONE',  ( 78.68120802659203150, 149.7457237375499517, -94.99999999999994316 ) ) ;
#4228 = DIRECTION ( 'NONE',  ( 0.000000000000000000, -1.000000000000000000, 0.000000000000000000 ) ) ;
#4229 = CARTESIAN_POINT ( 'NONE',  ( 2.416697501590669095, 172.9933428177121471, -50.00000000000000000 ) ) ;
#4230 = CARTESIAN_POINT ( 'NONE',  ( -11.93348319268873148, 448.8698905683720000, -2.051577885510841163E-15 ) ) ;
#4231 = VERTEX_POINT ( 'NONE', #13059 ) ;
#4232 = AXIS2_PLACEMENT_3D ( 'NONE', #11881, #3660, #16868 ) ;
#4233 = CARTESIAN_POINT ( 'NONE',  ( -10.20829729246299600, 451.6198905601784759, 7.653668647301790529 ) ) ;
#4234 = ORIENTED_EDGE ( 'NONE', *, *, #16908, .T. ) ;
#4235 = EDGE_LOOP ( 'NONE', ( #3141, #2166, #18379, #1030 ) ) ;
#4236 = ORIENTED_EDGE ( 'NONE', *, *, #179, .T. ) ;
#4237 = CARTESIAN_POINT ( 'NONE',  ( 81.24038404635966515, -343.0245277843623057, 94.99999999999994316 ) ) ;
#4238 = CARTESIAN_POINT ( 'NONE',  ( -47.16347859291443712, 316.6198905601784759, -7.653668647301793193 ) ) ;
#4239 = CARTESIAN_POINT ( 'NONE',  ( -44.16309181155855867, 294.4948905683720000, 6.410867750099241924 ) ) ;
#4240 = CARTESIAN_POINT ( 'NONE',  ( -38.17536295476244845, 356.9323905683720000, 14.20200298773971781 ) ) ;
#4241 = FACE_OUTER_BOUND ( 'NONE', #3204, .T. ) ;
#4242 = CARTESIAN_POINT ( 'NONE',  ( 91.21585410611801592, 56.85652257517428865, -40.00000000000000000 ) ) ;
#4243 = CARTESIAN_POINT ( 'NONE',  ( -38.17536295476245556, 405.4323905683721136, 14.20200298773971781 ) ) ;
#4244 = CARTESIAN_POINT ( 'NONE',  ( -42.88789093042841927, 246.3073905683720284, 9.489475012073736337 ) ) ;
#4245 = AXIS2_PLACEMENT_3D ( 'NONE', #13600, #303, #3321 ) ;
#4246 = CARTESIAN_POINT ( 'NONE',  ( -22.27502019258949062, 400.7448905683720568, -15.47720386886985544 ) ) ;
#4247 = CARTESIAN_POINT ( 'NONE',  ( -36.33955658999051508, 343.8698905765656377, 18.47759065022572500 ) ) ;
#4248 = CARTESIAN_POINT ( 'NONE',  ( -45.64106924314017277, 326.3073905601784759, -11.32908994701042538 ) ) ;
#4249 = CARTESIAN_POINT ( 'NONE',  ( -11.93348319268871371, 298.8698905683720000, -2.051577885510841163E-15 ) ) ;
#4250 = CARTESIAN_POINT ( 'NONE',  ( -28.68588794268872277, 457.8698905683720000, 16.75240474999999307 ) ) ;
#4251 = CARTESIAN_POINT ( 'NONE',  ( -28.68588794268872988, 514.4948905765655809, 19.99999999999999289 ) ) ;
#4252 = DIRECTION ( 'NONE',  ( 0.000000000000000000, 0.000000000000000000, 1.000000000000000000 ) ) ;
#4253 = CARTESIAN_POINT ( 'NONE',  ( 0.000000000000000000, 0.000000000000000000, 0.000000000000000000 ) ) ;
#4254 = ADVANCED_FACE ( 'NONE', ( #6341 ), #7319, .F. ) ;
#4255 = CARTESIAN_POINT ( 'NONE',  ( -14.48388495494899963, 369.4323905683720000, 9.489475012073732785 ) ) ;
#4256 = CARTESIAN_POINT ( 'NONE',  ( -11.93348319268873858, 508.5573905683720000, 3.332260488124728415 ) ) ;
#4257 = CARTESIAN_POINT ( 'NONE',  ( -40.01497788969916058, 515.6823905601784190, -16.95518130045146421 ) ) ;
#4258 = CARTESIAN_POINT ( 'NONE',  ( -32.01814843081344719, 351.6823905683720000, -16.75240474999999307 ) ) ;
#4259 = VERTEX_POINT ( 'NONE', #3218 ) ;
#4260 = CARTESIAN_POINT ( 'NONE',  ( -14.48388495494901562, 497.9323905683720568, 9.489475012073732785 ) ) ;
#4261 = ORIENTED_EDGE ( 'NONE', *, *, #20722, .F. ) ;
#4262 = EDGE_CURVE ( 'NONE', #13474, #18564, #18024, .T. ) ;
#4263 = CARTESIAN_POINT ( 'NONE',  ( -40.01497788969912506, 313.5573905765655809, 16.95518130045146776 ) ) ;
#4264 = CARTESIAN_POINT ( 'NONE',  ( -14.48388495494900674, 421.3073905683720000, -9.489475012073734561 ) ) ;
#4265 = LINE ( 'NONE', #7172, #4839 ) ;
#4266 = CARTESIAN_POINT ( 'NONE',  ( -11.73070664223726922, 517.9323905765655809, -11.32908994701042538 ) ) ;
#4267 = CARTESIAN_POINT ( 'NONE',  ( -19.19641293061499709, 470.4323905683719431, -14.20200298773971603 ) ) ;
#4268 = ORIENTED_EDGE ( 'NONE', *, *, #15151, .T. ) ;
#4269 = CARTESIAN_POINT ( 'NONE',  ( -45.43829269268872650, 463.8698905683720000, 0.000000000000000000 ) ) ;
#4270 = CARTESIAN_POINT ( 'NONE',  ( -48.68588794268873698, 573.2448905601785327, 0.000000000000000000 ) ) ;
#4271 = AXIS2_PLACEMENT_3D ( 'NONE', #6247, #21180, #19137 ) ;
#4272 = CARTESIAN_POINT ( 'NONE',  ( -48.68588794268871567, 401.6823905765655809, -3.978247347593158345 ) ) ;
#4273 = CARTESIAN_POINT ( 'NONE',  ( -54.57497958038185715, 230.5765313837437418, 25.00000000000000000 ) ) ;
#4274 = ADVANCED_FACE ( 'NONE', ( #9589 ), #14586, .F. ) ;
#4275 = DIRECTION ( 'NONE',  ( 1.000000000000000000, 0.000000000000000000, -0.000000000000000000 ) ) ;
#4276 = CARTESIAN_POINT ( 'NONE',  ( 82.89408817951444064, 286.0648460576640559, 40.00000000000000000 ) ) ;
#4277 = CARTESIAN_POINT ( 'NONE',  ( 14.09825962131072785, 160.1716627696692683, 25.00000000000000000 ) ) ;
#4278 = VECTOR ( 'NONE', #15277, 1000.000000000000114 ) ;
#4279 = CARTESIAN_POINT ( 'NONE',  ( 0.000000000000000000, -5.629165124598843661, 3.250000000000012434 ) ) ;
#4280 = CARTESIAN_POINT ( 'NONE',  ( 28.16023193154655502, 323.8848358243226357, 20.00000000000000355 ) ) ;
#4281 = CARTESIAN_POINT ( 'NONE',  ( -45.60737594483680368, 223.9102039777115749, 2.249240700863258002 ) ) ;
#4282 = CARTESIAN_POINT ( 'NONE',  ( -38.17536295476244135, 276.9323905683720000, 14.20200298773971781 ) ) ;
#4283 = ADVANCED_FACE ( 'NONE', ( #12636 ), #2794, .T. ) ;
#4284 = CARTESIAN_POINT ( 'NONE',  ( -36.33955658999050087, 249.1198905601784759, 18.47759065022572500 ) ) ;
#4285 = CARTESIAN_POINT ( 'NONE',  ( 5.674999999999999822, 0.000000000000000000, 0.000000000000000000 ) ) ;
#4286 = CARTESIAN_POINT ( 'NONE',  ( -14.48388495494900496, 419.4323905683720568, 9.489475012073732785 ) ) ;
#4287 = LINE ( 'NONE', #12510, #17174 ) ;
#4288 = CARTESIAN_POINT ( 'NONE',  ( -28.68588794268869790, 257.8698905683720000, 16.75240474999999307 ) ) ;
#4289 = VERTEX_POINT ( 'NONE', #1179 ) ;
#4290 = ORIENTED_EDGE ( 'NONE', *, *, #13282, .T. ) ;
#4291 = VERTEX_POINT ( 'NONE', #4825 ) ;
#4292 = CARTESIAN_POINT ( 'NONE',  ( -38.17536295476246266, 486.9323905683720568, 14.20200298773971781 ) ) ;
#4293 = ORIENTED_EDGE ( 'NONE', *, *, #12135, .T. ) ;
#4294 = CARTESIAN_POINT ( 'NONE',  ( -8.685887942688742314, 573.2448905601785327, 2.449293598294706119E-15 ) ) ;
#4295 = CARTESIAN_POINT ( 'NONE',  ( -28.68588794268869790, 246.3698905683720000, 16.75240474999999307 ) ) ;
#4296 = ORIENTED_EDGE ( 'NONE', *, *, #300, .T. ) ;
#4297 = CARTESIAN_POINT ( 'NONE',  ( -42.88789093042845479, 524.8073905683720568, 9.489475012073734561 ) ) ;
#4298 = DIRECTION ( 'NONE',  ( -1.000000000000000000, 0.000000000000000000, 0.000000000000000000 ) ) ;
#4299 = EDGE_CURVE ( 'NONE', #6189, #2640, #2625, .T. ) ;
#4300 = CARTESIAN_POINT ( 'NONE',  ( -11.73070664223726212, 457.9323905765655809, -11.32908994701042715 ) ) ;
#4301 = CARTESIAN_POINT ( 'NONE',  ( -32.66413529028186957, 349.4323905601785327, 19.99999999999999289 ) ) ;
#4302 = FACE_OUTER_BOUND ( 'NONE', #2059, .T. ) ;
#4303 = DIRECTION ( 'NONE',  ( -0.000000000000000000, -1.000000000000000000, -0.000000000000000000 ) ) ;
#4304 = DIRECTION ( 'NONE',  ( 0.000000000000000000, 0.000000000000000000, 1.000000000000000000 ) ) ;
#4305 = CARTESIAN_POINT ( 'NONE',  ( -28.68588794268872988, 507.8698905683720568, 16.75240474999999307 ) ) ;
#4306 = CARTESIAN_POINT ( 'NONE',  ( -28.68588794268873698, -129.7637193493918915, 0.000000000000000000 ) ) ;
#4307 = CARTESIAN_POINT ( 'NONE',  ( -40.53162694259542320, 235.1198905683720000, 11.84573899990672885 ) ) ;
#4308 = CARTESIAN_POINT ( 'NONE',  ( -19.19641293061498288, 331.9323905683720000, -14.20200298773971603 ) ) ;
#4309 = EDGE_CURVE ( 'NONE', #4929, #11681, #1275, .T. ) ;
#4310 = CARTESIAN_POINT ( 'NONE',  ( -11.73070664223724080, 321.3073905601784190, 11.32908994701042005 ) ) ;
#4311 = CARTESIAN_POINT ( 'NONE',  ( -11.93348319268872260, 378.5573905683721136, 3.332260488124728415 ) ) ;
#4312 = DIRECTION ( 'NONE',  ( -0.4627175328665442677, 0.000000000000000000, 0.8865057725575725689 ) ) ;
#4313 = CARTESIAN_POINT ( 'NONE',  ( -48.68588794268870856, 377.2448905601784759, 0.000000000000000000 ) ) ;
#4314 = EDGE_LOOP ( 'NONE', ( #16670, #13987, #14510, #12809 ) ) ;
#4315 = CARTESIAN_POINT ( 'NONE',  ( -1.025382690249029949, 213.9102039777116602, 25.00000000000000000 ) ) ;
#4316 = ORIENTED_EDGE ( 'NONE', *, *, #11546, .F. ) ;
#4317 = VERTEX_POINT ( 'NONE', #11215 ) ;
#4318 = CARTESIAN_POINT ( 'NONE',  ( -45.43829269268872650, 515.6823905683720568, 3.332260488124734632 ) ) ;
#4319 = CARTESIAN_POINT ( 'NONE',  ( -21.03221929538690205, 295.1198905765656377, 18.47759065022572500 ) ) ;
#4320 = ORIENTED_EDGE ( 'NONE', *, *, #20004, .T. ) ;
#4321 = CARTESIAN_POINT ( 'NONE',  ( -14.48388495494899075, 309.4323905683720568, 9.489475012073731008 ) ) ;
#4322 = VERTEX_POINT ( 'NONE', #6233 ) ;
#4323 = CARTESIAN_POINT ( 'NONE',  ( -40.53162694259543031, 325.1198905683720568, 11.84573899990672885 ) ) ;
#4324 = CARTESIAN_POINT ( 'NONE',  ( -16.84014894278198682, 340.1198905683720568, -11.84573899990672707 ) ) ;
#4325 = CARTESIAN_POINT ( 'NONE',  ( -10.20829729246297468, 257.6198905765656377, -7.653668647301794969 ) ) ;
#4326 = CARTESIAN_POINT ( 'NONE',  ( -14.54375231895777354, 393.4948905601784190, -14.14213562373094746 ) ) ;
#4327 = CARTESIAN_POINT ( 'NONE',  ( -28.68588794268870146, 251.3698905683720000, -16.75240474999999307 ) ) ;
#4328 = CARTESIAN_POINT ( 'NONE',  ( -28.68588794268869790, 224.7448905601784759, -19.99999999999999289 ) ) ;
#4329 = CARTESIAN_POINT ( 'NONE',  ( -40.53162694259544452, 406.6198905683720568, 11.84573899990672885 ) ) ;
#4330 = CARTESIAN_POINT ( 'NONE',  ( -28.68588794268871212, 334.7448905601784759, -19.99999999999999289 ) ) ;
#4331 = PLANE ( 'NONE',  #5548 ) ;
#4332 = EDGE_CURVE ( 'NONE', #15817, #11167, #19437, .T. ) ;
#4333 =( BOUNDED_CURVE ( )  B_SPLINE_CURVE ( 2, ( #7930, #12931, #20719, #4697, #176, #20059, #8366, #1465, #16501, #13466, #3406, #3615, #5234, #6415, #19951, #8141, #11511 ),
 .UNSPECIFIED., .F., .T. ) 
 B_SPLINE_CURVE_WITH_KNOTS ( ( 3, 2, 2, 2, 2, 2, 2, 2, 3 ),
 ( 0.3593750000000001110, 0.3613281250000001110, 0.3632812500000001110, 0.3652343750000001110, 0.3671875000000001110, 0.3691406250000001665, 0.3710937500000001665, 0.3730468750000001665, 0.3750000000000001665 ),
 .UNSPECIFIED. ) 
 CURVE ( )  GEOMETRIC_REPRESENTATION_ITEM ( )  RATIONAL_B_SPLINE_CURVE ( ( 0.9999999999999988898, 0.9807852804032315408, 1.000000000000000000, 0.9807852804032304306, 1.000000000000000000, 0.9807852804032304306, 1.000000000000000000, 0.9807852804032304306, 1.000000000000000000, 0.9807852804032304306, 1.000000000000000000, 0.9807852804032304306, 1.000000000000000000, 0.9807852804032304306, 1.000000000000000000, 0.9807852804032287652, 1.000000000000001554 ) ) 
 REPRESENTATION_ITEM ( '' )  );
#4334 = CARTESIAN_POINT ( 'NONE',  ( -48.68588794268869435, 247.2448905601785043, 0.000000000000000000 ) ) ;
#4335 = EDGE_CURVE ( 'NONE', #6728, #10701, #7955, .T. ) ;
#4336 = CARTESIAN_POINT ( 'NONE',  ( -11.93348319268872970, 438.5573905683720000, 3.332260488124728415 ) ) ;
#4337 = ORIENTED_EDGE ( 'NONE', *, *, #6785, .F. ) ;
#4338 = CARTESIAN_POINT ( 'NONE',  ( -8.685887942688729879, 442.5573905601784759, -3.978247347593165895 ) ) ;
#4339 = VERTEX_POINT ( 'NONE', #16635 ) ;
#4340 = ORIENTED_EDGE ( 'NONE', *, *, #20691, .T. ) ;
#4341 = PRODUCT_DEFINITION ( 'UNKNOWN', '', #13173, #2078 ) ;
#4342 = ORIENTED_EDGE ( 'NONE', *, *, #777, .T. ) ;
#4343 = CARTESIAN_POINT ( 'NONE',  ( 60.03793209889851568, 10.52886280891152104, 131.1729372809869005 ) ) ;
#4344 = CARTESIAN_POINT ( 'NONE',  ( -36.33955658999050797, 329.1198905601784759, 18.47759065022572500 ) ) ;
#4345 = CARTESIAN_POINT ( 'NONE',  ( -25.35362745456399125, 372.5573905683720568, -16.75240474999999307 ) ) ;
#4346 = CARTESIAN_POINT ( 'NONE',  ( 5.299999999999999822, -3.752776749732576356, -6.499999999999999112 ) ) ;
#4347 = CARTESIAN_POINT ( 'NONE',  ( -45.64106924314020119, 511.0573905765656946, -11.32908994701042715 ) ) ;
#4348 = CARTESIAN_POINT ( 'NONE',  ( -13.20868407381886200, 388.2448905683720000, 6.410867750099229490 ) ) ;
#4349 = CARTESIAN_POINT ( 'NONE',  ( -16.84014894278197261, 249.1198905683720284, 11.84573899990672530 ) ) ;
#4350 = CARTESIAN_POINT ( 'NONE',  ( -44.16309181155857289, 404.4948905683720000, 6.410867750099241924 ) ) ;
#4351 = CARTESIAN_POINT ( 'NONE',  ( -10.20829729246298356, 336.3698905765656377, 7.653668647301790529 ) ) ;
#4352 = FACE_BOUND ( 'NONE', #5166, .T. ) ;
#4353 = CARTESIAN_POINT ( 'NONE',  ( -22.27502019258946930, 306.9948905683720568, 15.47720386886985189 ) ) ;
#4354 = CARTESIAN_POINT ( 'NONE',  ( -40.53162694259545162, 466.6198905683720000, 11.84573899990672885 ) ) ;
#4355 = CARTESIAN_POINT ( 'NONE',  ( 20.42502041961813219, 290.7078131342035476, -7.833137205859951102 ) ) ;
#4356 = LINE ( 'NONE', #20694, #12994 ) ;
#4357 = CARTESIAN_POINT ( 'NONE',  ( -11.93348319268872082, 360.3698905683720568, -2.051577885510841163E-15 ) ) ;
#4358 = CARTESIAN_POINT ( 'NONE',  ( -16.84014894278200813, 510.1198905683720568, -11.84573899990672707 ) ) ;
#4359 = MANIFOLD_SOLID_BREP ( 'Cut-Extrude11', #5200 ) ;
#4360 = CARTESIAN_POINT ( 'NONE',  ( -45.64106924314020119, 498.1823905601784759, 11.32908994701042715 ) ) ;
#4361 = CARTESIAN_POINT ( 'NONE',  ( -13.20868407381885312, 318.2448905683720000, 6.410867750099229490 ) ) ;
#4362 = VECTOR ( 'NONE', #1875, 1000.000000000000114 ) ;
#4363 = VERTEX_POINT ( 'NONE', #1709 ) ;
#4364 = CARTESIAN_POINT ( 'NONE',  ( -42.88789093042844769, 494.8073905683720000, 9.489475012073736337 ) ) ;
#4365 = ORIENTED_EDGE ( 'NONE', *, *, #520, .F. ) ;
#4366 = DIRECTION ( 'NONE',  ( 1.000000000000000000, 0.000000000000000000, 0.000000000000000000 ) ) ;
#4367 = AXIS2_PLACEMENT_3D ( 'NONE', #19101, #20724, #18658 ) ;
#4368 = CARTESIAN_POINT ( 'NONE',  ( -44.16309181155857999, 424.7448905683720000, -6.410867750099231266 ) ) ;
#4369 = CARTESIAN_POINT ( 'NONE',  ( -8.685887942688735208, 472.2448905601784759, -2.449293598294705724E-15 ) ) ;
#4370 = SURFACE_STYLE_USAGE ( .BOTH. , #19191 ) ;
#4371 = CARTESIAN_POINT ( 'NONE',  ( -13.20868407381887089, 458.2448905683720568, 6.410867750099229490 ) ) ;
#4372 = ORIENTED_EDGE ( 'NONE', *, *, #15849, .F. ) ;
#4373 = CARTESIAN_POINT ( 'NONE',  ( -40.53162694259545162, 465.1198905683720568, 11.84573899990672885 ) ) ;
#4374 = CYLINDRICAL_SURFACE ( 'NONE', #9640, 4.000000000000001776 ) ;
#4375 = CARTESIAN_POINT ( 'NONE',  ( -11.73070664223725501, 407.9323905765656377, -11.32908994701042715 ) ) ;
#4376 = DIRECTION ( 'NONE',  ( 0.000000000000000000, -1.000000000000000000, 0.000000000000000000 ) ) ;
#4377 = LINE ( 'NONE', #20827, #2671 ) ;
#4378 = LINE ( 'NONE', #20605, #6332 ) ;
#4379 = DIRECTION ( 'NONE',  ( 0.000000000000000000, -1.000000000000000000, 0.000000000000000000 ) ) ;
#4380 = ADVANCED_FACE ( 'NONE', ( #13492 ), #8391, .T. ) ;
#4381 = AXIS2_PLACEMENT_3D ( 'NONE', #18322, #15099, #5236 ) ;
#4382 = CARTESIAN_POINT ( 'NONE',  ( 6.416697501590670427, 172.9933428177121471, 45.00000000000000000 ) ) ;
#4383 = CARTESIAN_POINT ( 'NONE',  ( -45.64106924314016567, 256.3073905601784759, -11.32908994701042538 ) ) ;
#4384 = ADVANCED_FACE ( 'NONE', ( #2031 ), #11751, .T. ) ;
#4385 = CARTESIAN_POINT ( 'NONE',  ( -45.46835912530129065, 223.9102039777117170, 4.966902868867238752 ) ) ;
#4386 = CARTESIAN_POINT ( 'NONE',  ( -40.01497788969911795, 238.8073905601784759, 16.95518130045146776 ) ) ;
#4387 = AXIS2_PLACEMENT_3D ( 'NONE', #9664, #8472, #8251 ) ;
#4388 = DIRECTION ( 'NONE',  ( 0.000000000000000000, 0.000000000000000000, 1.000000000000000000 ) ) ;
#4389 = CARTESIAN_POINT ( 'NONE',  ( -45.43829269268871229, 435.6823905683720568, 3.332260488124734632 ) ) ;
#4390 = CARTESIAN_POINT ( 'NONE',  ( -45.64106924314017988, 386.3073905601785327, -11.32908994701042538 ) ) ;
#4391 = CARTESIAN_POINT ( 'NONE',  ( -42.88789093042841927, 256.3073905683720568, 9.489475012073736337 ) ) ;
#4392 = ORIENTED_EDGE ( 'NONE', *, *, #1284, .F. ) ;
#4393 = ORIENTED_EDGE ( 'NONE', *, *, #14386, .T. ) ;
#4394 = DIRECTION ( 'NONE',  ( -1.000000000000000000, 0.000000000000000000, 0.000000000000000000 ) ) ;
#4395 = ORIENTED_EDGE ( 'NONE', *, *, #6483, .T. ) ;
#4396 = CARTESIAN_POINT ( 'NONE',  ( -28.68588794268872988, 462.8698905683720000, -16.75240474999999307 ) ) ;
#4397 = VECTOR ( 'NONE', #9456, 1000.000000000000000 ) ;
#4398 = VERTEX_POINT ( 'NONE', #6550 ) ;
#4399 = PLANE ( 'NONE',  #16960 ) ;
#4400 = CARTESIAN_POINT ( 'NONE',  ( -28.68588794268870146, 231.3698905683720284, -16.75240474999999307 ) ) ;
#4401 = ORIENTED_EDGE ( 'NONE', *, *, #11019, .F. ) ;
#4402 = CARTESIAN_POINT ( 'NONE',  ( -16.84014894278200458, 517.6198905683719431, 11.84573899990672530 ) ) ;
#4403 = DIRECTION ( 'NONE',  ( 0.000000000000000000, 0.5000000000000008882, -0.8660254037844380415 ) ) ;
#4404 = ADVANCED_FACE ( 'NONE', ( #18347 ), #11538, .F. ) ;
#4405 = AXIS2_PLACEMENT_3D ( 'NONE', #17423, #5835, #10696 ) ;
#4406 = CARTESIAN_POINT ( 'NONE',  ( -24.70764059509557242, 459.1823905765656377, -19.99999999999999289 ) ) ;
#4407 = PRODUCT ( 'Heavy Arch Steel Frame Casting', 'Heavy Arch Steel Frame Casting', '', ( #18096 ) ) ;
#4408 = CARTESIAN_POINT ( 'NONE',  ( -42.82802356641965957, 348.4948905601785327, 14.14213562373094923 ) ) ;
#4409 = CARTESIAN_POINT ( 'NONE',  ( 40.42502041961814996, 180.1716627696692967, 20.00000000000000355 ) ) ;
#4410 = CARTESIAN_POINT ( 'NONE',  ( -23.03786159879532036, 223.9102039777118023, -18.55174335541752839 ) ) ;
#4411 = DIRECTION ( 'NONE',  ( -1.191790137725560488E-16, 1.000000000000000000, -0.000000000000000000 ) ) ;
#4412 = CARTESIAN_POINT ( 'NONE',  ( -40.53162694259542320, 232.6198905683720000, -11.84573899990672707 ) ) ;
#4413 = CARTESIAN_POINT ( 'NONE',  ( -14.48388495494899431, 329.4323905683720568, 9.489475012073732785 ) ) ;
#4414 = CARTESIAN_POINT ( 'NONE',  ( -8.685887942688893304, 321.9323905601784190, 3.978247347593586447 ) ) ;
#4415 = CARTESIAN_POINT ( 'NONE',  ( 5.421010862427523403E-17, 0.6351314446054991958, 6.500000000000000888 ) ) ;
#4416 = CARTESIAN_POINT ( 'NONE',  ( -32.01814843081344009, 303.1823905683720000, -16.75240474999999307 ) ) ;
#4417 = ADVANCED_FACE ( 'NONE', ( #10122 ), #15222, .F. ) ;
#4418 = CARTESIAN_POINT ( 'NONE',  ( -45.43829269268870519, 383.5573905683720000, -3.332260488124726194 ) ) ;
#4419 = CARTESIAN_POINT ( 'NONE',  ( -19.19641293061500420, 521.9323905683720568, -14.20200298773971603 ) ) ;
#4420 = CARTESIAN_POINT ( 'NONE',  ( -11.73070664223724968, 381.3073905601784759, 11.32908994701042005 ) ) ;
#4421 = CARTESIAN_POINT ( 'NONE',  ( -24.70764059509556176, 404.4323905601785327, -19.99999999999999289 ) ) ;
#4422 = EDGE_LOOP ( 'NONE', ( #13095, #13480 ) ) ;
#4423 = ORIENTED_EDGE ( 'NONE', *, *, #2159, .F. ) ;
#4424 = CARTESIAN_POINT ( 'NONE',  ( -38.17536295476246977, 506.9323905683720568, 14.20200298773971781 ) ) ;
#4425 = CARTESIAN_POINT ( 'NONE',  ( -24.70764059509554045, 294.8073905765655809, 19.99999999999998934 ) ) ;
#4426 = ORIENTED_EDGE ( 'NONE', *, *, #3235, .F. ) ;
#4427 = EDGE_CURVE ( 'NONE', #15324, #604, #15123, .T. ) ;
#4428 = CARTESIAN_POINT ( 'NONE',  ( -14.48388495494899253, 301.3073905683720000, -9.489475012073734561 ) ) ;
#4429 = CARTESIAN_POINT ( 'NONE',  ( -45.43829269268869808, 324.1823905683720000, 3.332260488124734632 ) ) ;
#4430 = CARTESIAN_POINT ( 'NONE',  ( -28.68588794268870501, 269.4948905765656377, -19.99999999999999289 ) ) ;
#4431 = CARTESIAN_POINT ( 'NONE',  ( -21.03221929538692692, 394.1198905601784759, -18.47759065022572855 ) ) ;
#4432 = CARTESIAN_POINT ( 'NONE',  ( -28.68588794268869790, 236.3698905683720568, 16.75240474999999307 ) ) ;
#4433 = DIRECTION ( 'NONE',  ( 1.000000000000000000, 0.000000000000000000, 0.000000000000000000 ) ) ;
#4434 = CARTESIAN_POINT ( 'NONE',  ( -11.93348319268872437, 390.0573905683720568, 3.332260488124728415 ) ) ;
#4435 = CARTESIAN_POINT ( 'NONE',  ( 77.07016797226398808, 161.6844911138030056, 40.00000000000000000 ) ) ;
#4436 = CARTESIAN_POINT ( 'NONE',  ( -54.57497958038185004, 303.6587712403113528, 49.99999999999999289 ) ) ;
#4437 = PLANE ( 'NONE',  #4937 ) ;
#4438 = AXIS2_PLACEMENT_3D ( 'NONE', #17598, #1173, #14374 ) ;
#4439 = CARTESIAN_POINT ( 'NONE',  ( -44.16309181155857289, 434.4948905683720568, 6.410867750099241924 ) ) ;
#4440 = ORIENTED_EDGE ( 'NONE', *, *, #17782, .F. ) ;
#4441 = CARTESIAN_POINT ( 'NONE',  ( -21.03221929538693402, 444.1198905601784759, -18.47759065022572855 ) ) ;
#4442 = VERTEX_POINT ( 'NONE', #6874 ) ;
#4443 = ORIENTED_EDGE ( 'NONE', *, *, #4335, .T. ) ;
#4444 = ORIENTED_EDGE ( 'NONE', *, *, #13069, .F. ) ;
#4445 = CARTESIAN_POINT ( 'NONE',  ( -28.68588794268872988, 10.52886280891152104, -49.60091809715359545 ) ) ;
#4446 = CARTESIAN_POINT ( 'NONE',  ( -32.66413529028186957, 329.4323905601784759, 19.99999999999999289 ) ) ;
#4447 = PLANE ( 'NONE',  #8269 ) ;
#4448 = CARTESIAN_POINT ( 'NONE',  ( -42.88789093042843348, 364.4323905683720000, -9.489475012073734561 ) ) ;
#4449 = DIRECTION ( 'NONE',  ( 0.000000000000000000, 0.000000000000000000, 1.000000000000000000 ) ) ;
#4450 = CARTESIAN_POINT ( 'NONE',  ( -45.64106924314020119, 512.9323905765656946, 11.32908994701042715 ) ) ;
#4451 = CARTESIAN_POINT ( 'NONE',  ( -25.35362745456399480, 391.0573905683720568, -16.75240474999999307 ) ) ;
#4452 = FACE_BOUND ( 'NONE', #15353, .T. ) ;
#4453 = EDGE_CURVE ( 'NONE', #21078, #13633, #5181, .T. ) ;
#4454 = CARTESIAN_POINT ( 'NONE',  ( -44.16309181155857999, 413.2448905683720568, -6.410867750099231266 ) ) ;
#4455 = CARTESIAN_POINT ( 'NONE',  ( -11.73070664223724791, 327.9323905765656377, -11.32908994701042715 ) ) ;
#4456 = DIRECTION ( 'NONE',  ( 0.000000000000000000, 0.000000000000000000, 1.000000000000000000 ) ) ;
#4457 = CARTESIAN_POINT ( 'NONE',  ( -45.43829269268870519, 313.5573905683720000, -3.332260488124726638 ) ) ;
#4458 = SHAPE_REPRESENTATION_RELATIONSHIP ( 'NONE' , 'NONE' ,  #18847, #4042 ) ;
#4459 =( BOUNDED_CURVE ( )  B_SPLINE_CURVE ( 2, ( #8640, #15267, #449, #7016, #8854, #5612, #20225, #12105, #552, #15475, #13846, #12000, #12220, #18590, #10364, #3986, #10577 ),
 .UNSPECIFIED., .F., .T. ) 
 B_SPLINE_CURVE_WITH_KNOTS ( ( 3, 2, 2, 2, 2, 2, 2, 2, 3 ),
 ( 0.6562500000000002220, 0.6582031250000002220, 0.6601562500000002220, 0.6621093750000002220, 0.6640625000000002220, 0.6660156250000002220, 0.6679687500000002220, 0.6699218750000002220, 0.6718750000000002220 ),
 .UNSPECIFIED. ) 
 CURVE ( )  GEOMETRIC_REPRESENTATION_ITEM ( )  RATIONAL_B_SPLINE_CURVE ( ( 0.9999999999999977796, 0.9807852804032326510, 1.000000000000000000, 0.9807852804032304306, 1.000000000000000000, 0.9807852804032304306, 1.000000000000000000, 0.9807852804032304306, 1.000000000000000000, 0.9807852804032304306, 1.000000000000000000, 0.9807852804032304306, 1.000000000000000000, 0.9807852804032304306, 1.000000000000000000, 0.9807852804032282101, 1.000000000000002220 ) ) 
 REPRESENTATION_ITEM ( '' )  );
#4460 = CARTESIAN_POINT ( 'NONE',  ( -16.84014894278199748, 459.1198905683720568, 11.84573899990672530 ) ) ;
#4461 = CARTESIAN_POINT ( 'NONE',  ( -33.07955326574332133, 600.7448905601785327, 10.74819839862556492 ) ) ;
#4462 = CARTESIAN_POINT ( 'NONE',  ( 0.000000000000000000, 30.52886280891154058, 0.000000000000000000 ) ) ;
#4463 = CARTESIAN_POINT ( 'NONE',  ( 52.60622592008805043, 30.52886280891152282, 151.0302712373927250 ) ) ;
#4464 = EDGE_CURVE ( 'NONE', #683, #13710, #15626, .T. ) ;
#4465 = CARTESIAN_POINT ( 'NONE',  ( -32.01814843081344719, 363.1823905683720568, -16.75240474999999307 ) ) ;
#4466 = CARTESIAN_POINT ( 'NONE',  ( -22.27502019258950128, 510.7448905683720000, -15.47720386886985544 ) ) ;
#4467 =( REPRESENTATION_RELATIONSHIP ('NONE','NONE', #1888, #3392 ) REPRESENTATION_RELATIONSHIP_WITH_TRANSFORMATION ( #12144 )SHAPE_REPRESENTATION_RELATIONSHIP( ) );
#4468 = EDGE_CURVE ( 'NONE', #983, #554, #8710, .T. ) ;
#4469 = CARTESIAN_POINT ( 'NONE',  ( -8.685887942688738761, 512.2448905601784190, -2.449293598294705724E-15 ) ) ;
#4470 = CARTESIAN_POINT ( 'NONE',  ( -35.09675569278794427, 325.7448905683720000, 15.47720386886985366 ) ) ;
#4471 = AXIS2_PLACEMENT_3D ( 'NONE', #9738, #1431, #17959 ) ;
#4472 = EDGE_CURVE ( 'NONE', #18084, #13236, #14014, .T. ) ;
#4473 = ORIENTED_EDGE ( 'NONE', *, *, #1603, .F. ) ;
#4474 = CARTESIAN_POINT ( 'NONE',  ( 0.06682554136337748307, 4.993536075455418555, -4.350941807883111245 ) ) ;
#4475 = ORIENTED_EDGE ( 'NONE', *, *, #11277, .T. ) ;
#4476 = DIRECTION ( 'NONE',  ( -1.191790137725560488E-16, 1.000000000000000000, -0.000000000000000000 ) ) ;
#4477 = CARTESIAN_POINT ( 'NONE',  ( -19.19641293061498644, 418.8073905683720000, 14.20200298773971426 ) ) ;
#4478 = CARTESIAN_POINT ( 'NONE',  ( -17.35679799567829207, 395.4323905765655809, 16.95518130045146421 ) ) ;
#4479 = DIRECTION ( 'NONE',  ( -1.000000000000000000, 0.000000000000000000, 0.000000000000000000 ) ) ;
#4480 = CARTESIAN_POINT ( 'NONE',  ( -14.48388495494900852, 449.8073905683720000, -9.489475012073736337 ) ) ;
#4481 = EDGE_LOOP ( 'NONE', ( #21096, #20626, #19086, #11523 ) ) ;
#4482 = CARTESIAN_POINT ( 'NONE',  ( -13.20868407381887444, 469.4948905683720000, -6.410867750099233042 ) ) ;
#4483 = DIRECTION ( 'NONE',  ( -0.000000000000000000, 1.000000000000000000, -0.000000000000000000 ) ) ;
#4484 = ADVANCED_FACE ( 'NONE', ( #18654, #17264, #13808 ), #15545, .F. ) ;
#4485 = CARTESIAN_POINT ( 'NONE',  ( -28.68588794268871567, 374.4948905765656377, 19.99999999999999289 ) ) ;
#4486 = FACE_OUTER_BOUND ( 'NONE', #1336, .T. ) ;
#4487 = CARTESIAN_POINT ( 'NONE',  ( -8.685887942688740537, 522.2448905601784190, -2.449293598294705724E-15 ) ) ;
#4488 = DIRECTION ( 'NONE',  ( -1.191790137725560488E-16, 1.000000000000000000, -0.000000000000000000 ) ) ;
#4489 = LINE ( 'NONE', #12925, #9062 ) ;
#4490 = VECTOR ( 'NONE', #9418, 1000.000000000000000 ) ;
#4491 = CARTESIAN_POINT ( 'NONE',  ( -8.685887942688731655, 452.2448905601784759, -2.449293598294705724E-15 ) ) ;
#4492 = FACE_OUTER_BOUND ( 'NONE', #9286, .T. ) ;
#4493 = CARTESIAN_POINT ( 'NONE',  ( 71.32175588950862277, 75.31183677523708297, -94.99999999999994316 ) ) ;
#4494 = CARTESIAN_POINT ( 'NONE',  ( -13.20868407381886556, 419.7448905683720000, 6.410867750099229490 ) ) ;
#4495 = CARTESIAN_POINT ( 'NONE',  ( -28.68588794268875475, 600.7448905601785327, 0.000000000000000000 ) ) ;
#4496 = CARTESIAN_POINT ( 'NONE',  ( -45.43829269268869098, 245.6823905683720284, 3.332260488124734632 ) ) ;
#4497 = VERTEX_POINT ( 'NONE', #20609 ) ;
#4498 = CARTESIAN_POINT ( 'NONE',  ( -49.57497958038185715, 160.1716627696692683, -60.00000000000000000 ) ) ;
#4499 = ORIENTED_EDGE ( 'NONE', *, *, #17031, .F. ) ;
#4500 = CARTESIAN_POINT ( 'NONE',  ( -11.93348319268873503, 470.6823905683720000, -3.332260488124732856 ) ) ;
#4501 = CARTESIAN_POINT ( 'NONE',  ( -32.66413529028186247, 219.8073905765656377, -19.99999999999999289 ) ) ;
#4502 =( GEOMETRIC_REPRESENTATION_CONTEXT ( 3 ) GLOBAL_UNCERTAINTY_ASSIGNED_CONTEXT ( ( #18501 ) ) GLOBAL_UNIT_ASSIGNED_CONTEXT ( ( #9106, #19067, #15620 ) ) REPRESENTATION_CONTEXT ( 'NONE', 'WORKASPACE' ) );
#4503 = ORIENTED_EDGE ( 'NONE', *, *, #3832, .T. ) ;
#4504 = DIRECTION ( 'NONE',  ( -1.191790137725560488E-16, 1.000000000000000000, -0.000000000000000000 ) ) ;
#4505 = CARTESIAN_POINT ( 'NONE',  ( -32.01814843081343298, 226.0573905683720568, 16.75240474999999307 ) ) ;
#4506 = ORIENTED_EDGE ( 'NONE', *, *, #3168, .T. ) ;
#4508 = MANIFOLD_SOLID_BREP ( 'Boss-Extrude6', #2450 ) ;
#4507 = CARTESIAN_POINT ( 'NONE',  ( -45.43829269268873361, 533.8698905683720568, 0.000000000000000000 ) ) ;
#4509 = FACE_OUTER_BOUND ( 'NONE', #1394, .T. ) ;
#4510 = AXIS2_PLACEMENT_3D ( 'NONE', #851, #5908, #17483 ) ;
#4511 = CARTESIAN_POINT ( 'NONE',  ( -11.73070664223726389, 467.9323905765655809, -11.32908994701042715 ) ) ;
#4512 = DIRECTION ( 'NONE',  ( -1.000000000000000000, -0.000000000000000000, 0.000000000000000000 ) ) ;
#4513 = CARTESIAN_POINT ( 'NONE',  ( -8.685887942688712116, 276.9948905765656377, -2.449293598294705724E-15 ) ) ;
#4514 = CARTESIAN_POINT ( 'NONE',  ( -10.20829729246297291, 237.6198905765656377, -7.653668647301794969 ) ) ;
#4515 = FACE_OUTER_BOUND ( 'NONE', #9042, .T. ) ;
#4516 =( NAMED_UNIT ( * ) SI_UNIT ( $, .STERADIAN. ) SOLID_ANGLE_UNIT ( ) );
#4517 = CARTESIAN_POINT ( 'NONE',  ( -45.43829269268869098, 223.5573905683720284, -3.332260488124726194 ) ) ;
#4518 = CARTESIAN_POINT ( 'NONE',  ( -16.84014894278198327, 319.1198905683720568, 11.84573899990672530 ) ) ;
#4519 = DIRECTION ( 'NONE',  ( 0.000000000000000000, 0.000000000000000000, -1.000000000000000000 ) ) ;
#4520 = CARTESIAN_POINT ( 'NONE',  ( 0.000000000000000000, -343.0245277843623057, 0.000000000000000000 ) ) ;
#4521 = CARTESIAN_POINT ( 'NONE',  ( -22.27502019258947996, 312.2448905683720000, -15.47720386886985544 ) ) ;
#4522 = EDGE_CURVE ( 'NONE', #8747, #13873, #2156, .T. ) ;
#4523 = VECTOR ( 'NONE', #12179, 1000.000000000000114 ) ;
#4524 = CARTESIAN_POINT ( 'NONE',  ( -22.27502019258947996, 386.9948905683720568, 15.47720386886985189 ) ) ;
#4525 = AXIS2_PLACEMENT_3D ( 'NONE', #4747, #17940, #1850 ) ;
#4526 = CARTESIAN_POINT ( 'NONE',  ( -32.01814843081346140, 533.1823905683720568, -16.75240474999999307 ) ) ;
#4527 = CARTESIAN_POINT ( 'NONE',  ( -48.68588794268870856, 367.5573905601785327, 3.978247347593168115 ) ) ;
#4528 = CARTESIAN_POINT ( 'NONE',  ( -48.68588794268872277, 497.2448905601785327, 0.000000000000000000 ) ) ;
#4529 = EDGE_LOOP ( 'NONE', ( #16668, #4268 ) ) ;
#4530 = CARTESIAN_POINT ( 'NONE',  ( -44.16309181155857999, 485.9948905683720568, 6.410867750099241924 ) ) ;
#4531 = PRODUCT_RELATED_PRODUCT_CATEGORY ( 'part', '', ( #8019 ) ) ;
#4532 = CYLINDRICAL_SURFACE ( 'NONE', #6955, 19.99999999999999645 ) ;
#4533 = VECTOR ( 'NONE', #10141, 1000.000000000000000 ) ;
#4534 = ORIENTED_EDGE ( 'NONE', *, *, #11651, .F. ) ;
#4535 = CARTESIAN_POINT ( 'NONE',  ( -32.01814843081344009, 293.1823905683720568, -16.75240474999999307 ) ) ;
#4536 = CARTESIAN_POINT ( 'NONE',  ( -11.93348319268871727, 319.1823905683720568, -3.332260488124732856 ) ) ;
#4537 = EDGE_CURVE ( 'NONE', #1608, #20007, #17602, .T. ) ;
#4538 = AXIS2_PLACEMENT_3D ( 'NONE', #11685, #21311, #1861 ) ;
#4539 = CARTESIAN_POINT ( 'NONE',  ( -45.64106924314017277, 261.0573905765656377, -11.32908994701042715 ) ) ;
#4540 = CARTESIAN_POINT ( 'NONE',  ( 52.60622592008805043, 10.52886280891152104, 151.0302712373927250 ) ) ;
#4541 = CARTESIAN_POINT ( 'NONE',  ( -14.48388495494898187, 227.9323905683720000, 9.489475012073731008 ) ) ;
#4542 = CARTESIAN_POINT ( 'NONE',  ( -18.66955214161060894, 223.9106467678502383, -17.31106641270412183 ) ) ;
#4543 = CARTESIAN_POINT ( 'NONE',  ( -22.27502019258947996, 378.4948905683720000, 15.47720386886985189 ) ) ;
#4544 = CARTESIAN_POINT ( 'NONE',  ( -43.67481775055303928, 200.1767262095909246, 0.6600471188826699809 ) ) ;
#4545 = DIRECTION ( 'NONE',  ( 1.000000000000000000, 0.000000000000000000, 0.000000000000000000 ) ) ;
#4546 = EDGE_CURVE ( 'NONE', #19853, #5504, #15755, .T. ) ;
#4547 = CARTESIAN_POINT ( 'NONE',  ( -25.35362745456399125, 446.6823905683720568, 16.75240474999998952 ) ) ;
#4548 = FACE_OUTER_BOUND ( 'NONE', #6531, .T. ) ;
#4549 = EDGE_LOOP ( 'NONE', ( #1804, #11307, #4815, #14469 ) ) ;
#4550 = CARTESIAN_POINT ( 'NONE',  ( -21.03221929538691981, 450.3698905601784759, 18.47759065022572500 ) ) ;
#4551 = VERTEX_POINT ( 'NONE', #9246 ) ;
#4552 = ORIENTED_EDGE ( 'NONE', *, *, #14782, .T. ) ;
#4553 = CARTESIAN_POINT ( 'NONE',  ( -42.91697296918459159, 206.7606908932681051, -4.742769269235594720 ) ) ;
#4554 = AXIS2_PLACEMENT_3D ( 'NONE', #19903, #10051, #19477 ) ;
#4555 = CARTESIAN_POINT ( 'NONE',  ( -32.66413529028187668, 335.0573905601784759, -19.99999999999999289 ) ) ;
#4556 = LINE ( 'NONE', #2835, #4490 ) ;
#4557 = VECTOR ( 'NONE', #15783, 999.9999999999998863 ) ;
#4558 = CARTESIAN_POINT ( 'NONE',  ( -22.27502019258948707, 372.2448905683720000, -15.47720386886985544 ) ) ;
#4559 = DIRECTION ( 'NONE',  ( 1.000000000000000000, 0.000000000000000000, 0.000000000000000000 ) ) ;
#4560 = CARTESIAN_POINT ( 'NONE',  ( -47.16347859291445843, 502.6198905765656377, 7.653668647301805628 ) ) ;
#4561 = CARTESIAN_POINT ( 'NONE',  ( -45.43829269268871229, 394.1823905683720000, 3.332260488124734632 ) ) ;
#4562 = CARTESIAN_POINT ( 'NONE',  ( -32.01814843081343298, 227.5573905683720568, 16.75240474999999307 ) ) ;
#4563 = CARTESIAN_POINT ( 'NONE',  ( -19.19641293061498288, 377.3073905683721136, 14.20200298773971426 ) ) ;
#4564 = CARTESIAN_POINT ( 'NONE',  ( -40.01497788969913216, 333.5573905765655240, 16.95518130045146776 ) ) ;
#4565 = CARTESIAN_POINT ( 'NONE',  ( 105.7989814974898479, 142.5259582928263455, 20.00000000000000355 ) ) ;
#4566 = CARTESIAN_POINT ( 'NONE',  ( -32.01814843081344009, 286.0573905683720568, 16.75240474999999307 ) ) ;
#4567 = CARTESIAN_POINT ( 'NONE',  ( -35.09675569278795848, 453.4948905683720568, -15.47720386886985544 ) ) ;
#4568 = CARTESIAN_POINT ( 'NONE',  ( -42.82802356641967378, 458.4948905601784759, 14.14213562373094923 ) ) ;
#4569 = LINE ( 'NONE', #1127, #14559 ) ;
#4570 = LINE ( 'NONE', #17446, #20607 ) ;
#4571 = AXIS2_PLACEMENT_3D ( 'NONE', #9094, #2510, #7683 ) ;
#4572 = CARTESIAN_POINT ( 'NONE',  ( -13.20868407381886023, 369.7448905683720568, 6.410867750099229490 ) ) ;
#4573 = CARTESIAN_POINT ( 'NONE',  ( -45.43829269268871940, 493.5573905683720568, -3.332260488124726194 ) ) ;
#4574 = CARTESIAN_POINT ( 'NONE',  ( -45.64106924314020119, 506.3073905601784759, -11.32908994701042715 ) ) ;
#4575 = CARTESIAN_POINT ( 'NONE',  ( -16.84014894278198682, 320.1198905683720568, -11.84573899990672707 ) ) ;
#4576 = EDGE_LOOP ( 'NONE', ( #7682, #10156, #19212, #2994 ) ) ;
#4577 = CARTESIAN_POINT ( 'NONE',  ( -47.16347859291443001, 257.8698905601785327, 7.653668647301805628 ) ) ;
#4578 = ORIENTED_EDGE ( 'NONE', *, *, #11471, .F. ) ;
#4579 = AXIS2_PLACEMENT_3D ( 'NONE', #8036, #10967, #17575 ) ;
#4580 = DIRECTION ( 'NONE',  ( -1.232945044042657126E-32, 9.855701800883825964E-17, 1.000000000000000000 ) ) ;
#4581 = CARTESIAN_POINT ( 'NONE',  ( -40.53162694259544452, 426.6198905683720000, 11.84573899990672885 ) ) ;
#4582 = CARTESIAN_POINT ( 'NONE',  ( -48.68588794268869435, 231.9948905765656377, 0.000000000000000000 ) ) ;
#4583 = CARTESIAN_POINT ( 'NONE',  ( -11.93348319268872970, 438.5573905683720000, 3.332260488124728415 ) ) ;
#4584 = VERTEX_POINT ( 'NONE', #12065 ) ;
#4585 = CARTESIAN_POINT ( 'NONE',  ( -22.27502019258949773, 460.7448905683720568, -15.47720386886985544 ) ) ;
#4586 = CARTESIAN_POINT ( 'NONE',  ( 35.96497763894179656, 170.1716627696692683, 57.37501161332323107 ) ) ;
#4587 = CARTESIAN_POINT ( 'NONE',  ( -42.82802356641965957, 383.2448905765656377, 14.14213562373094923 ) ) ;
#4588 = FACE_OUTER_BOUND ( 'NONE', #17325, .T. ) ;
#4589 = FACE_OUTER_BOUND ( 'NONE', #1990, .T. ) ;
#4590 = CARTESIAN_POINT ( 'NONE',  ( 0.2578475836320679448, 4.367703157927326885, -5.434916218090832807 ) ) ;
#4591 = CARTESIAN_POINT ( 'NONE',  ( -8.685887942688886199, 256.6823905765655809, 3.978247347593586447 ) ) ;
#4592 = EDGE_CURVE ( 'NONE', #2137, #18782, #10424, .T. ) ;
#4593 = ADVANCED_FACE ( 'NONE', ( #1153 ), #16179, .F. ) ;
#4594 = FACE_OUTER_BOUND ( 'NONE', #15211, .T. ) ;
#4595 = CARTESIAN_POINT ( 'NONE',  ( 158.8141120573112630, 610.7448905601785327, 0.000000000000000000 ) ) ;
#4596 = CARTESIAN_POINT ( 'NONE',  ( -39.91673061078817852, 223.9102039777116886, 15.70339761151467606 ) ) ;
#4597 = CONICAL_SURFACE ( 'NONE', #3228, 6.500000000000000000, 1.047197551196600296 ) ;
#4598 = CARTESIAN_POINT ( 'NONE',  ( -44.16309181155857289, 435.9948905683720568, 6.410867750099241924 ) ) ;
#4599 = FACE_BOUND ( 'NONE', #6370, .T. ) ;
#4600 = CARTESIAN_POINT ( 'NONE',  ( -19.19641293061497223, 241.9323905683720284, -14.20200298773971603 ) ) ;
#4601 = EDGE_CURVE ( 'NONE', #5209, #6223, #6630, .T. ) ;
#4602 = ORIENTED_EDGE ( 'NONE', *, *, #3842, .T. ) ;
#4603 = ORIENTED_EDGE ( 'NONE', *, *, #19059, .F. ) ;
#4604 = FACE_OUTER_BOUND ( 'NONE', #3799, .T. ) ;
#4605 = EDGE_LOOP ( 'NONE', ( #4072, #4113, #13010, #15980 ) ) ;
#4606 = CARTESIAN_POINT ( 'NONE',  ( -11.93348319268873503, 470.0573905683720568, 3.332260488124728859 ) ) ;
#4607 = CARTESIAN_POINT ( 'NONE',  ( -11.73070664223723369, 227.9323905765656662, -11.32908994701042715 ) ) ;
#4608 = CIRCLE ( 'NONE', #16715, 43.46661168214937732 ) ;
#4609 = ORIENTED_EDGE ( 'NONE', *, *, #14084, .T. ) ;
#4610 = CARTESIAN_POINT ( 'NONE',  ( 29.72350413846044859, 280.4463447002762564, -20.00000000000000355 ) ) ;
#4611 = CARTESIAN_POINT ( 'NONE',  ( -14.48388495494901917, 531.3073905683719431, -9.489475012073736337 ) ) ;
#4612 = ORIENTED_EDGE ( 'NONE', *, *, #18880, .T. ) ;
#4613 = CARTESIAN_POINT ( 'NONE',  ( -13.68588794268869435, 188.9102039777116602, 1.836970198721029983E-15 ) ) ;
#4614 = DIRECTION ( 'NONE',  ( 0.000000000000000000, 0.000000000000000000, -1.000000000000000000 ) ) ;
#4615 = CARTESIAN_POINT ( 'NONE',  ( -17.35679799567830983, 448.5573905765656946, -16.95518130045146421 ) ) ;
#4616 = CARTESIAN_POINT ( 'NONE',  ( 0.4042117618287677239, -3.141900367811078620, 6.500000000000001776 ) ) ;
#4617 = CARTESIAN_POINT ( 'NONE',  ( -28.68588794268874054, 573.2448905601785327, 0.000000000000000000 ) ) ;
#4618 = FACE_BOUND ( 'NONE', #16556, .T. ) ;
#4619 = DIRECTION ( 'NONE',  ( 1.000000000000000000, 1.191790137725560488E-16, 0.000000000000000000 ) ) ;
#4620 = CARTESIAN_POINT ( 'NONE',  ( 80.02941346738570871, 139.7547175612648402, 70.25248122596298117 ) ) ;
#4621 = CARTESIAN_POINT ( 'NONE',  ( -28.68588794268869790, 236.3698905683720568, 16.75240474999999307 ) ) ;
#4622 = CARTESIAN_POINT ( 'NONE',  ( -11.93348319268871727, 310.0573905683720568, 3.332260488124728415 ) ) ;
#4623 = AXIS2_PLACEMENT_3D ( 'NONE', #18751, #4580, #12804 ) ;
#4624 = CARTESIAN_POINT ( 'NONE',  ( -36.33955658999049376, 235.3698905601784759, -18.47759065022572855 ) ) ;
#4625 = CARTESIAN_POINT ( 'NONE',  ( -48.68588794268870856, 377.2448905601784759, 0.000000000000000000 ) ) ;
#4626 = CIRCLE ( 'NONE', #7381, 49.60091809715359545 ) ;
#4627 = CARTESIAN_POINT ( 'NONE',  ( -11.93348319268871371, 300.3698905683720568, -2.051577885510841163E-15 ) ) ;
#4628 = CARTESIAN_POINT ( 'NONE',  ( -44.16309181155857289, 363.2448905683720000, -6.410867750099231266 ) ) ;
#4629 = CARTESIAN_POINT ( 'NONE',  ( -35.09675569278797269, 527.2448905683719431, 15.47720386886985366 ) ) ;
#4630 = CARTESIAN_POINT ( 'NONE',  ( -11.73070664223725146, 363.1823905601784759, -11.32908994701042715 ) ) ;
#4631 = CARTESIAN_POINT ( 'NONE',  ( -47.16347859291445133, 406.6198905601784759, -7.653668647301793193 ) ) ;
#4632 = ORIENTED_EDGE ( 'NONE', *, *, #14597, .F. ) ;
#4633 = CARTESIAN_POINT ( 'NONE',  ( -14.48388495494901385, 489.4323905683720568, 9.489475012073732785 ) ) ;
#4634 = DIRECTION ( 'NONE',  ( -1.191790137725560488E-16, 1.000000000000000000, -0.000000000000000000 ) ) ;
#4635 = CARTESIAN_POINT ( 'NONE',  ( -22.27502019258946930, 286.9948905683720000, 15.47720386886985189 ) ) ;
#4636 = VERTEX_POINT ( 'NONE', #7725 ) ;
#4637 = CARTESIAN_POINT ( 'NONE',  ( -13.20868407381884779, 279.7448905683720568, 6.410867750099229490 ) ) ;
#4638 = CARTESIAN_POINT ( 'NONE',  ( -32.01814843081344009, 316.0573905683720000, 16.75240474999999307 ) ) ;
#4639 = CARTESIAN_POINT ( 'NONE',  ( -13.20868407381884779, 260.9948905683720568, -6.410867750099233042 ) ) ;
#4640 = VECTOR ( 'NONE', #8021, 1000.000000000000000 ) ;
#4641 = ADVANCED_FACE ( 'NONE', ( #4492 ), #9352, .T. ) ;
#4642 = CARTESIAN_POINT ( 'NONE',  ( -21.03221929538689849, 255.1198905765656377, 18.47759065022572500 ) ) ;
#4643 = CARTESIAN_POINT ( 'NONE',  ( 28.16023193154655502, 323.8848358243226357, -20.00000000000000355 ) ) ;
#4644 = CARTESIAN_POINT ( 'NONE',  ( -45.43280446313950449, 223.9102039777116602, 0.4287796227366179602 ) ) ;
#4645 = CARTESIAN_POINT ( 'NONE',  ( -13.20868407381886023, 369.7448905683720568, 6.410867750099229490 ) ) ;
#4646 = LINE ( 'NONE', #16443, #16857 ) ;
#4647 = CARTESIAN_POINT ( 'NONE',  ( -18.68588794268873698, 281.1055109169419666, 20.00000000000000355 ) ) ;
#4648 = EDGE_CURVE ( 'NONE', #5794, #18805, #752, .T. ) ;
#4649 = DIRECTION ( 'NONE',  ( 0.000000000000000000, -1.000000000000000000, 0.000000000000000000 ) ) ;
#4650 = CARTESIAN_POINT ( 'NONE',  ( -45.43829269268871940, 433.8698905683720568, 0.000000000000000000 ) ) ;
#4651 = DIRECTION ( 'NONE',  ( 0.000000000000000000, 0.000000000000000000, 1.000000000000000000 ) ) ;
#4652 = EDGE_LOOP ( 'NONE', ( #2597, #16221, #7909, #17273, #13763 ) ) ;
#4653 = CARTESIAN_POINT ( 'NONE',  ( -8.685887942688728103, 422.5573905601785327, -3.978247347593165895 ) ) ;
#4654 = ORIENTED_EDGE ( 'NONE', *, *, #15114, .F. ) ;
#4655 = ORIENTED_EDGE ( 'NONE', *, *, #7092, .T. ) ;
#4656 = ORIENTED_EDGE ( 'NONE', *, *, #17736, .F. ) ;
#4657 = CARTESIAN_POINT ( 'NONE',  ( -32.66413529028186957, 354.1823905765656377, 19.99999999999999289 ) ) ;
#4658 = CARTESIAN_POINT ( 'NONE',  ( -11.73070664223724613, 313.1823905601784190, -11.32908994701042715 ) ) ;
#4659 = DIRECTION ( 'NONE',  ( -1.000000000000000000, 0.000000000000000000, 0.000000000000000000 ) ) ;
#4660 = CARTESIAN_POINT ( 'NONE',  ( -13.20868407381885667, 339.7448905683720568, 6.410867750099229490 ) ) ;
#4661 = CARTESIAN_POINT ( 'NONE',  ( -17.35679799567831338, 498.5573905765655809, -16.95518130045146421 ) ) ;
#4662 = CARTESIAN_POINT ( 'NONE',  ( -19.19641293061498644, 377.3073905683720568, 14.20200298773971426 ) ) ;
#4663 = DIRECTION ( 'NONE',  ( 1.000000000000000000, 1.191790137725560488E-16, 0.000000000000000000 ) ) ;
#4664 = CARTESIAN_POINT ( 'NONE',  ( -45.43829269268871940, 394.1823905683720000, 3.332260488124734632 ) ) ;
#4665 = EDGE_CURVE ( 'NONE', #11550, #11897, #1464, .T. ) ;
#4666 = CARTESIAN_POINT ( 'NONE',  ( -8.685887942688715668, 316.6823905765655240, 3.978247347593161010 ) ) ;
#4667 = CARTESIAN_POINT ( 'NONE',  ( -11.73070664223725679, 423.1823905601785327, -11.32908994701042538 ) ) ;
#4668 = CARTESIAN_POINT ( 'NONE',  ( -13.20868407381885135, 289.4948905683720000, -6.410867750099233042 ) ) ;
#4669 = CARTESIAN_POINT ( 'NONE',  ( -25.35362745456400191, 442.5573905683720568, -16.75240474999999307 ) ) ;
#4670 = CARTESIAN_POINT ( 'NONE',  ( -43.68588794268869435, 213.9102039777116602, 0.000000000000000000 ) ) ;
#4671 = CARTESIAN_POINT ( 'NONE',  ( 32.47532367400565079, 600.7448905601785327, -163.9643442751439864 ) ) ;
#4672 = CYLINDRICAL_SURFACE ( 'NONE', #6080, 19.99999999999999645 ) ;
#4673 = CARTESIAN_POINT ( 'NONE',  ( -14.48388495494899608, 339.4323905683720000, 9.489475012073732785 ) ) ;
#4674 = CARTESIAN_POINT ( 'NONE',  ( -40.53162694259545873, 512.6198905683720568, -11.84573899990672707 ) ) ;
#4675 = CARTESIAN_POINT ( 'NONE',  ( -42.82802356641967378, 495.9948905601784759, -14.14213562373094746 ) ) ;
#4676 = CARTESIAN_POINT ( 'NONE',  ( -45.43829269268869808, 323.5573905683720000, -3.332260488124726194 ) ) ;
#4677 = EDGE_CURVE ( 'NONE', #4217, #15177, #8039, .T. ) ;
#4678 = ORIENTED_EDGE ( 'NONE', *, *, #1355, .F. ) ;
#4679 = CARTESIAN_POINT ( 'NONE',  ( -48.68588794268886488, 257.5573905601784190, 3.978247347592742678 ) ) ;
#4680 = ORIENTED_EDGE ( 'NONE', *, *, #11128, .F. ) ;
#4681 = CARTESIAN_POINT ( 'NONE',  ( -18.68588794268873698, 281.1055109169419666, -20.00000000000000355 ) ) ;
#4682 = CARTESIAN_POINT ( 'NONE',  ( -28.68588794268871922, 402.8698905683720000, -16.75240474999999307 ) ) ;
#4683 = CARTESIAN_POINT ( 'NONE',  ( -21.03221929538689849, 235.1198905765656377, 18.47759065022572500 ) ) ;
#4684 = CARTESIAN_POINT ( 'NONE',  ( -44.16309181155858710, 453.2448905683720000, -6.410867750099231266 ) ) ;
#4685 = CARTESIAN_POINT ( 'NONE',  ( -11.93348319268873148, 448.8698905683720000, -2.051577885510841163E-15 ) ) ;
#4686 = DIRECTION ( 'NONE',  ( 0.000000000000000000, 0.000000000000000000, 1.000000000000000000 ) ) ;
#4687 = CARTESIAN_POINT ( 'NONE',  ( 0.000000000000000000, 31.85652257517428865, 0.000000000000000000 ) ) ;
#4688 = EDGE_CURVE ( 'NONE', #14788, #11298, #12823, .T. ) ;
#4689 = CARTESIAN_POINT ( 'NONE',  ( -32.66413529028188378, 389.8073905765656377, -19.99999999999999289 ) ) ;
#4690 = CARTESIAN_POINT ( 'NONE',  ( -23.30554231582819469, 45.34767784731757700, 49.31100188924479966 ) ) ;
#4691 = CARTESIAN_POINT ( 'NONE',  ( -71.26501780185373036, 130.1716627696692683, 25.00000000000000000 ) ) ;
#4692 = CARTESIAN_POINT ( 'NONE',  ( -10.20829729246299422, 427.6198905765656377, -7.653668647301794969 ) ) ;
#4693 = DIRECTION ( 'NONE',  ( 0.000000000000000000, -1.000000000000000000, 0.000000000000000000 ) ) ;
#4694 = CARTESIAN_POINT ( 'NONE',  ( -42.88789093042844769, 496.3073905683720568, 9.489475012073736337 ) ) ;
#4695 = CARTESIAN_POINT ( 'NONE',  ( -8.685887942688742314, 573.2448905601785327, 2.449293598294706119E-15 ) ) ;
#4696 = CARTESIAN_POINT ( 'NONE',  ( 147.4234352242185935, 620.7448905601785327, 1.893624729818134345 ) ) ;
#4697 = CARTESIAN_POINT ( 'NONE',  ( -11.73070664223725323, 421.3073905601784190, 11.32908994701042005 ) ) ;
#4698 = CARTESIAN_POINT ( 'NONE',  ( -35.09675569278795848, 407.2448905683720568, 15.47720386886985366 ) ) ;
#4699 = CARTESIAN_POINT ( 'NONE',  ( 30.42502041961813575, 271.1055109169419097, -20.00000000000000355 ) ) ;
#4700 = B_SPLINE_CURVE_WITH_KNOTS ( 'NONE', 3,
 ( #15113, #10114, #8490, #85, #6651, #8383, #5147, #15007, #8704, #10214, #11636, #5456, #297, #18231, #19858, #5035, #15326, #18646, #3423, #6866, #19968, #193, #10002, #18545, #13378, #20078, #12058, #20286, #3838, #16625, #1700, #16735, #11745, #1922, #11850, #11951, #18446, #3632, #16837, #407 ),
 .UNSPECIFIED., .F., .F.,
 ( 4, 2, 2, 2, 2, 2, 2, 2, 2, 2, 2, 2, 2, 2, 2, 2, 2, 2, 2, 4 ),
 ( 0.000000000000000000, 0.003131370304449435787, 0.004697055456674143273, 0.006262740608898849023, 0.007045583185011209705, 0.007828425761123570387, 0.009394110913348300423, 0.01095979606557302699, 0.01174263864168539201, 0.01252548121779775703, 0.01409116637002248706, 0.01487400894613485382, 0.01565685152224722057, 0.01878822182669671534, 0.01957106440280908730, 0.02035390697892145925, 0.02191959213114619623, 0.02270243470725856819, 0.02348527728337093667, 0.02505096243559567018 ),
 .UNSPECIFIED. ) ;
#4701 = CARTESIAN_POINT ( 'NONE',  ( -32.01814843081343298, 257.5573905683720568, 16.75240474999999307 ) ) ;
#4702 = ORIENTED_EDGE ( 'NONE', *, *, #16376, .F. ) ;
#4703 = DIRECTION ( 'NONE',  ( -1.000000000000000000, 0.000000000000000000, 0.000000000000000000 ) ) ;
#4704 = ORIENTED_EDGE ( 'NONE', *, *, #14132, .F. ) ;
#4705 = CARTESIAN_POINT ( 'NONE',  ( -42.88789093042844769, 466.3073905683721136, 9.489475012073734561 ) ) ;
#4706 = CARTESIAN_POINT ( 'NONE',  ( -24.70764059509552979, 224.8073905765656662, 19.99999999999998934 ) ) ;
#4707 = EDGE_LOOP ( 'NONE', ( #6643, #4951, #636, #18935 ) ) ;
#4708 = CARTESIAN_POINT ( 'NONE',  ( -40.01497788969915348, 523.5573905765656946, 16.95518130045146776 ) ) ;
#4709 = CARTESIAN_POINT ( 'NONE',  ( -22.27502019258949773, 528.4948905683719431, 15.47720386886985189 ) ) ;
#4710 = ORIENTED_EDGE ( 'NONE', *, *, #16903, .T. ) ;
#4711 = CARTESIAN_POINT ( 'NONE',  ( -11.93348319268873858, 499.1823905683720568, -3.332260488124732856 ) ) ;
#4712 = LINE ( 'NONE', #11309, #20013 ) ;
#4713 = CIRCLE ( 'NONE', #20967, 50.00000000000000000 ) ;
#4714 = CARTESIAN_POINT ( 'NONE',  ( -42.82802356641966668, 443.2448905765656377, 14.14213562373094923 ) ) ;
#4715 = CARTESIAN_POINT ( 'NONE',  ( -8.685887942688706786, 232.2448905601785043, -2.449293598294705724E-15 ) ) ;
#4716 = CARTESIAN_POINT ( 'NONE',  ( -25.35362745456397704, 336.6823905683720568, 16.75240474999998952 ) ) ;
#4717 =( LENGTH_UNIT ( ) NAMED_UNIT ( * ) SI_UNIT ( .MILLI., .METRE. ) );
#4718 = CARTESIAN_POINT ( 'NONE',  ( -28.68588794268874409, 600.7448905601785327, 0.000000000000000000 ) ) ;
#4719 = EDGE_CURVE ( 'NONE', #11194, #20333, #10390, .T. ) ;
#4720 = CARTESIAN_POINT ( 'NONE',  ( 20.42502041961813575, 271.1055109169419666, -40.00000000000000000 ) ) ;
#4721 = EDGE_CURVE ( 'NONE', #2882, #983, #14671, .T. ) ;
#4722 = DIRECTION ( 'NONE',  ( 1.191790137725560488E-16, -1.000000000000000000, -0.000000000000000000 ) ) ;
#4723 = DIRECTION ( 'NONE',  ( 0.000000000000000000, -0.000000000000000000, -1.000000000000000000 ) ) ;
#4724 = CARTESIAN_POINT ( 'NONE',  ( -25.35362745456398770, 322.5573905683720000, -16.75240474999999307 ) ) ;
#4725 = CARTESIAN_POINT ( 'NONE',  ( -40.01497788969914637, 445.6823905601784190, -16.95518130045146421 ) ) ;
#4726 = PRODUCT_RELATED_PRODUCT_CATEGORY ( 'part', '', ( #19431 ) ) ;
#4727 = CARTESIAN_POINT ( 'NONE',  ( -22.27502019258947286, 318.4948905683720000, 15.47720386886985189 ) ) ;
#4728 = AXIS2_PLACEMENT_3D ( 'NONE', #14008, #5443, #15518 ) ;
#4729 = CARTESIAN_POINT ( 'NONE',  ( -45.43829269268873361, 515.0573905683720568, -3.332260488124726638 ) ) ;
#4730 = CARTESIAN_POINT ( 'NONE',  ( -45.64106924314018698, 366.3073905601785327, -11.32908994701042715 ) ) ;
#4731 = VECTOR ( 'NONE', #15835, 1000.000000000000000 ) ;
#4732 = CARTESIAN_POINT ( 'NONE',  ( -48.68588794268872988, 521.9948905765656946, 0.000000000000000000 ) ) ;
#4733 = ORIENTED_EDGE ( 'NONE', *, *, #2098, .T. ) ;
#4734 = CARTESIAN_POINT ( 'NONE',  ( -11.93348319268873503, 480.3698905683720568, -2.051577885510841163E-15 ) ) ;
#4735 = DIRECTION ( 'NONE',  ( 0.000000000000000000, -1.000000000000000000, 0.000000000000000000 ) ) ;
#4736 = CARTESIAN_POINT ( 'NONE',  ( -11.93348319268871371, 288.5573905683720000, 3.332260488124728415 ) ) ;
#4737 = ORIENTED_EDGE ( 'NONE', *, *, #1693, .F. ) ;
#4738 = CARTESIAN_POINT ( 'NONE',  ( -19.19641293061497223, 288.8073905683719431, 14.20200298773971426 ) ) ;
#4739 = CARTESIAN_POINT ( 'NONE',  ( -38.17536295476244845, 322.3073905683720568, -14.20200298773971426 ) ) ;
#4740 = CARTESIAN_POINT ( 'NONE',  ( -38.17536295476243424, 266.9323905683720568, 14.20200298773971781 ) ) ;
#4741 = CARTESIAN_POINT ( 'NONE',  ( -42.82802356641964536, 260.7448905765656377, -14.14213562373094746 ) ) ;
#4742 = LINE ( 'NONE', #19775, #21056 ) ;
#4743 = CARTESIAN_POINT ( 'NONE',  ( -28.68588794268869435, 226.3698905683720284, 16.75240474999999307 ) ) ;
#4744 = CARTESIAN_POINT ( 'NONE',  ( -16.84014894278199037, 371.6198905683720000, -11.84573899990672707 ) ) ;
#4745 = VECTOR ( 'NONE', #1979, 1000.000000000000000 ) ;
#4746 = CARTESIAN_POINT ( 'NONE',  ( -162.2727221670389781, 30.52886280891152282, -20.57735571454641033 ) ) ;
#4747 = CARTESIAN_POINT ( 'NONE',  ( 5.299999999999999822, 0.000000000000000000, 0.000000000000000000 ) ) ;
#4748 = PRODUCT_DEFINITION_SHAPE ( 'NONE', 'NONE',  #21407 ) ;
#4749 = CARTESIAN_POINT ( 'NONE',  ( -14.31911992702480774, 585.7448905601785327, -19.70857778461545351 ) ) ;
#4750 = CARTESIAN_POINT ( 'NONE',  ( -11.93348319268872970, 429.1823905683720568, -3.332260488124732856 ) ) ;
#4751 = FACE_OUTER_BOUND ( 'NONE', #7459, .T. ) ;
#4752 = ORIENTED_EDGE ( 'NONE', *, *, #1121, .T. ) ;
#4753 = CARTESIAN_POINT ( 'NONE',  ( -32.66413529028188378, 435.0573905601784759, -19.99999999999999289 ) ) ;
#4754 = ORIENTED_EDGE ( 'NONE', *, *, #7166, .F. ) ;
#4755 = VERTEX_POINT ( 'NONE', #3192 ) ;
#4756 = ORIENTED_EDGE ( 'NONE', *, *, #21293, .T. ) ;
#4757 = CARTESIAN_POINT ( 'NONE',  ( -42.88446638378037079, 206.4484180351192322, -4.837872587287148640 ) ) ;
#4758 = CARTESIAN_POINT ( 'NONE',  ( -17.35679799567828496, 300.6823905601784759, 16.95518130045146421 ) ) ;
#4759 = FACE_OUTER_BOUND ( 'NONE', #5931, .T. ) ;
#4760 = CARTESIAN_POINT ( 'NONE',  ( -40.53162694259543741, 344.1198905683720568, -11.84573899990672707 ) ) ;
#4761 = EDGE_CURVE ( 'NONE', #14968, #17590, #19306, .T. ) ;
#4762 = CARTESIAN_POINT ( 'NONE',  ( -32.66413529028189089, 499.8073905765656377, -19.99999999999999289 ) ) ;
#4763 = CARTESIAN_POINT ( 'NONE',  ( -38.17536295476245556, 382.3073905683719431, -14.20200298773971426 ) ) ;
#4764 = CARTESIAN_POINT ( 'NONE',  ( -28.68588794268869790, 213.9102039777116602, 0.000000000000000000 ) ) ;
#4765 = CARTESIAN_POINT ( 'NONE',  ( -11.93348319268872260, 378.5573905683721136, 3.332260488124728859 ) ) ;
#4766 =( BOUNDED_CURVE ( )  B_SPLINE_CURVE ( 2, ( #12070, #18771, #3959, #10547, #5791, #2347, #10761, #15551, #843, #735, #7302, #12397, #18877, #4067, #10651, #17271, #14034 ),
 .UNSPECIFIED., .F., .T. ) 
 B_SPLINE_CURVE_WITH_KNOTS ( ( 3, 2, 2, 2, 2, 2, 2, 2, 3 ),
 ( 0.6250000000000002220, 0.6269531250000002220, 0.6289062500000002220, 0.6308593750000002220, 0.6328125000000002220, 0.6347656250000002220, 0.6367187500000002220, 0.6386718750000002220, 0.6406250000000002220 ),
 .UNSPECIFIED. ) 
 CURVE ( )  GEOMETRIC_REPRESENTATION_ITEM ( )  RATIONAL_B_SPLINE_CURVE ( ( 0.9999999999999977796, 0.9807852804032326510, 1.000000000000000000, 0.9807852804032304306, 1.000000000000000000, 0.9807852804032304306, 1.000000000000000000, 0.9807852804032304306, 1.000000000000000000, 0.9807852804032304306, 1.000000000000000000, 0.9807852804032304306, 1.000000000000000000, 0.9807852804032304306, 1.000000000000000000, 0.9807852804032282101, 1.000000000000002220 ) ) 
 REPRESENTATION_ITEM ( '' )  );
#4767 = CARTESIAN_POINT ( 'NONE',  ( -10.20829729246298179, 326.3698905765656377, 7.653668647301790529 ) ) ;
#4768 = PLANE ( 'NONE',  #10337 ) ;
#4769 = CARTESIAN_POINT ( 'NONE',  ( -44.16309181155856578, 283.2448905683720568, -6.410867750099231266 ) ) ;
#4770 = CARTESIAN_POINT ( 'NONE',  ( -40.53162694259544452, 444.1198905683720568, -11.84573899990672707 ) ) ;
#4771 = DIRECTION ( 'NONE',  ( 1.000000000000000000, 0.000000000000000000, 0.000000000000000000 ) ) ;
#4772 = DIRECTION ( 'NONE',  ( 0.000000000000000000, 1.000000000000000000, 0.000000000000000000 ) ) ;
#4773 = CARTESIAN_POINT ( 'NONE',  ( -42.82802356641964536, 205.1437886375728965, -5.000000000000001776 ) ) ;
#4774 = CARTESIAN_POINT ( 'NONE',  ( -45.43829269268870519, 345.6823905683720568, 3.332260488124734632 ) ) ;
#4775 = CARTESIAN_POINT ( 'NONE',  ( -44.16309181155858710, 473.2448905683720568, -6.410867750099231266 ) ) ;
#4776 = CARTESIAN_POINT ( 'NONE',  ( -48.68588794268872277, 476.9323905601784759, -3.978247347593158345 ) ) ;
#4777 = CARTESIAN_POINT ( 'NONE',  ( -25.35362745456397704, 326.6823905683720568, 16.75240474999998952 ) ) ;
#4778 = EDGE_CURVE ( 'NONE', #15582, #11085, #17685, .T. ) ;
#4779 = VERTEX_POINT ( 'NONE', #5333 ) ;
#4780 = DIRECTION ( 'NONE',  ( 0.000000000000000000, 0.000000000000000000, -1.000000000000000000 ) ) ;
#4781 = ORIENTED_EDGE ( 'NONE', *, *, #14481, .F. ) ;
#4782 = FACE_OUTER_BOUND ( 'NONE', #9469, .T. ) ;
#4783 = AXIS2_PLACEMENT_3D ( 'NONE', #12303, #5374, #19802 ) ;
#4784 = CARTESIAN_POINT ( 'NONE',  ( -28.68588794268871922, 407.8698905683720568, 16.75240474999999307 ) ) ;
#4785 = CARTESIAN_POINT ( 'NONE',  ( -28.68588794268874054, 573.2448905601785327, 0.000000000000000000 ) ) ;
#4786 = DIRECTION ( 'NONE',  ( 1.000000000000000000, 0.000000000000000000, -0.000000000000000000 ) ) ;
#4787 = CARTESIAN_POINT ( 'NONE',  ( -45.43829269268871940, 454.1823905683720568, 3.332260488124734632 ) ) ;
#4788 = CARTESIAN_POINT ( 'NONE',  ( -44.16309181155857289, 444.4948905683720568, 6.410867750099241924 ) ) ;
#4789 = DIRECTION ( 'NONE',  ( 0.000000000000000000, 0.000000000000000000, 1.000000000000000000 ) ) ;
#4790 = CARTESIAN_POINT ( 'NONE',  ( -48.68588794268858067, 416.9323905601784190, -3.978247347593477201 ) ) ;
#4791 = CARTESIAN_POINT ( 'NONE',  ( -48.68588794268870856, 381.6823905765656377, -3.978247347593158345 ) ) ;
#4792 = CARTESIAN_POINT ( 'NONE',  ( -10.76731745429010090, 56.85652257517428865, 46.25122601329427141 ) ) ;
#4793 = CARTESIAN_POINT ( 'NONE',  ( -24.70764059509554755, 264.4323905601784759, -19.99999999999999289 ) ) ;
#4794 = PLANE ( 'NONE',  #18083 ) ;
#4795 = DIRECTION ( 'NONE',  ( -0.000000000000000000, -0.000000000000000000, 1.000000000000000000 ) ) ;
#4796 = CARTESIAN_POINT ( 'NONE',  ( -13.20868407381887621, 499.7448905683720000, 6.410867750099229490 ) ) ;
#4797 = EDGE_CURVE ( 'NONE', #19523, #15642, #5970, .T. ) ;
#4798 = DIRECTION ( 'NONE',  ( 0.000000000000000000, 0.000000000000000000, 1.000000000000000000 ) ) ;
#4799 = DIRECTION ( 'NONE',  ( 1.000000000000000000, 0.000000000000000000, 2.399110633850889130E-16 ) ) ;
#4800 = CARTESIAN_POINT ( 'NONE',  ( 5.074999999999999289, -5.629165124598850767, -3.250000000000003109 ) ) ;
#4801 = VECTOR ( 'NONE', #15618, 1000.000000000000000 ) ;
#4802 = CARTESIAN_POINT ( 'NONE',  ( -14.48388495494900496, 411.3073905683720000, -9.489475012073736337 ) ) ;
#4803 = CARTESIAN_POINT ( 'NONE',  ( -32.66413529028188378, 469.8073905765656377, -19.99999999999999289 ) ) ;
#4804 = CARTESIAN_POINT ( 'NONE',  ( -35.09675569278793716, 227.2448905683720568, 15.47720386886985366 ) ) ;
#4805 = EDGE_CURVE ( 'NONE', #9261, #16878, #18427, .T. ) ;
#4806 = ORIENTED_EDGE ( 'NONE', *, *, #11450, .T. ) ;
#4807 = CARTESIAN_POINT ( 'NONE',  ( -47.16347859291445133, 422.6198905765656377, 7.653668647301805628 ) ) ;
#4808 = ORIENTED_EDGE ( 'NONE', *, *, #20677, .T. ) ;
#4809 = AXIS2_PLACEMENT_3D ( 'NONE', #15959, #8028, #17986 ) ;
#4810 = CARTESIAN_POINT ( 'NONE',  ( -13.20868407381887089, 469.7448905683720568, 6.410867750099229490 ) ) ;
#4811 = CARTESIAN_POINT ( 'NONE',  ( -21.03221929538689494, 225.1198905765656093, 18.47759065022572500 ) ) ;
#4812 = ORIENTED_EDGE ( 'NONE', *, *, #21337, .F. ) ;
#4813 = CARTESIAN_POINT ( 'NONE',  ( -43.04716123355245116, 207.6569251493015429, 4.334626618252812591 ) ) ;
#4814 = CARTESIAN_POINT ( 'NONE',  ( -32.01814843081346851, 527.5573905683720568, 16.75240474999999307 ) ) ;
#4815 = ORIENTED_EDGE ( 'NONE', *, *, #11157, .T. ) ;
#4816 = CARTESIAN_POINT ( 'NONE',  ( -35.09675569278797269, 515.7448905683720568, 15.47720386886985366 ) ) ;
#4817 = CARTESIAN_POINT ( 'NONE',  ( 0.2573354458087834251, 6.889406814520511624, -1.067197363239225316 ) ) ;
#4818 = VECTOR ( 'NONE', #2282, 999.9999999999998863 ) ;
#4819 = CARTESIAN_POINT ( 'NONE',  ( -40.01497788969913927, 443.5573905765656377, 16.95518130045146776 ) ) ;
#4820 = CARTESIAN_POINT ( 'NONE',  ( 60.03793209889851568, 10.52886280891152104, -131.1729372809869005 ) ) ;
#4821 = DIRECTION ( 'NONE',  ( -0.000000000000000000, -1.000000000000000000, -0.000000000000000000 ) ) ;
#4822 = CARTESIAN_POINT ( 'NONE',  ( -40.01497788969914637, 453.5573905765656377, 16.95518130045146776 ) ) ;
#4823 = DIRECTION ( 'NONE',  ( 1.000000000000000000, 0.000000000000000000, -0.000000000000000000 ) ) ;
#4824 = CARTESIAN_POINT ( 'NONE',  ( 0.000000000000000000, 0.000000000000000000, -40.00000000000000000 ) ) ;
#4825 = CARTESIAN_POINT ( 'NONE',  ( 171.3141120573112630, 575.7448905601785327, 0.000000000000000000 ) ) ;
#4826 = CARTESIAN_POINT ( 'NONE',  ( -15.76477386065954356, 223.9102039777117739, -15.36505724430687714 ) ) ;
#4827 = CARTESIAN_POINT ( 'NONE',  ( -35.09675569278793716, 323.4948905683720000, -15.47720386886985544 ) ) ;
#4828 = CARTESIAN_POINT ( 'NONE',  ( -8.685887942688642838, 442.5573905601784759, -3.978247347592952732 ) ) ;
#4829 = CARTESIAN_POINT ( 'NONE',  ( -45.64106924314017988, 276.3073905601785327, -11.32908994701042715 ) ) ;
#4830 = CARTESIAN_POINT ( 'NONE',  ( 154.7587007620219026, 620.7448905601785327, 10.81142786866622885 ) ) ;
#4831 = CARTESIAN_POINT ( 'NONE',  ( -44.16309181155855867, 285.9948905683720000, 6.410867750099241924 ) ) ;
#4832 = CARTESIAN_POINT ( 'NONE',  ( -38.17536295476247687, 523.8073905683720568, -14.20200298773971426 ) ) ;
#4833 = CARTESIAN_POINT ( 'NONE',  ( -36.33955658999051508, 359.1198905601785327, 18.47759065022572500 ) ) ;
#4834 = DIRECTION ( 'NONE',  ( 0.000000000000000000, 1.000000000000000000, 0.000000000000000000 ) ) ;
#4835 = ORIENTED_EDGE ( 'NONE', *, *, #17610, .T. ) ;
#4836 = CARTESIAN_POINT ( 'NONE',  ( -38.17536295476246266, 486.9323905683721136, 14.20200298773971781 ) ) ;
#4837 = DIRECTION ( 'NONE',  ( 0.000000000000000000, 0.000000000000000000, 1.000000000000000000 ) ) ;
#4838 = CARTESIAN_POINT ( 'NONE',  ( -35.09675569278793716, 281.9948905683720000, -15.47720386886985544 ) ) ;
#4839 = VECTOR ( 'NONE', #17456, 1000.000000000000000 ) ;
#4840 = ORIENTED_EDGE ( 'NONE', *, *, #3638, .F. ) ;
#4841 = CARTESIAN_POINT ( 'NONE',  ( -44.16309181155855867, 275.9948905683720000, 6.410867750099241924 ) ) ;
#4842 = CARTESIAN_POINT ( 'NONE',  ( -45.43829269268870519, 313.8698905683720000, 0.000000000000000000 ) ) ;
#4843 = EDGE_CURVE ( 'NONE', #7864, #16350, #20058, .T. ) ;
#4844 = CARTESIAN_POINT ( 'NONE',  ( -17.35679799567828496, 238.5573905765656093, -16.95518130045146421 ) ) ;
#4845 = AXIS2_PLACEMENT_3D ( 'NONE', #10960, #19298, #7716 ) ;
#4846 = CARTESIAN_POINT ( 'NONE',  ( -48.68588794268870146, 321.9948905765655809, 0.000000000000000000 ) ) ;
#4847 = LINE ( 'NONE', #17626, #6463 ) ;
#4848 = EDGE_CURVE ( 'NONE', #12430, #14255, #11832, .T. ) ;
#4849 = CARTESIAN_POINT ( 'NONE',  ( -16.84014894278199037, 379.1198905683720568, 11.84573899990672530 ) ) ;
#4850 = EDGE_CURVE ( 'NONE', #4363, #16962, #16500, .T. ) ;
#4851 = FACE_OUTER_BOUND ( 'NONE', #17407, .T. ) ;
#4852 = VECTOR ( 'NONE', #19216, 1000.000000000000000 ) ;
#4853 = AXIS2_PLACEMENT_3D ( 'NONE', #19384, #19178, #2954 ) ;
#4854 = CARTESIAN_POINT ( 'NONE',  ( -40.01497788969915348, 460.4323905765656377, -16.95518130045146421 ) ) ;
#4855 = VECTOR ( 'NONE', #5854, 1000.000000000000000 ) ;
#4856 = CARTESIAN_POINT ( 'NONE',  ( -48.68588794268853803, 271.6823905765656377, -3.978247347593583783 ) ) ;
#4857 = CARTESIAN_POINT ( 'NONE',  ( -22.27502019258949417, 420.7448905683720000, -15.47720386886985544 ) ) ;
#4858 = UNCERTAINTY_MEASURE_WITH_UNIT (LENGTH_MEASURE( 1.000000000000000082E-05 ), #4717, 'distance_accuracy_value', 'NONE');
#4859 = CARTESIAN_POINT ( 'NONE',  ( 5.074999999999999289, -5.629165124598844550, 3.250000000000012434 ) ) ;
#4860 = ORIENTED_EDGE ( 'NONE', *, *, #18010, .F. ) ;
#4861 = CARTESIAN_POINT ( 'NONE',  ( -11.73070664223725679, 423.1823905601784759, -11.32908994701042715 ) ) ;
#4862 = EDGE_CURVE ( 'NONE', #11055, #502, #19950, .T. ) ;
#4863 = ORIENTED_EDGE ( 'NONE', *, *, #16944, .F. ) ;
#4864 = CARTESIAN_POINT ( 'NONE',  ( -22.27502019258947641, 262.2448905683720000, -15.47720386886985544 ) ) ;
#4865 = DIRECTION ( 'NONE',  ( -1.000000000000000000, 0.000000000000000000, 0.000000000000000000 ) ) ;
#4866 = VERTEX_POINT ( 'NONE', #15096 ) ;
#4867 = ORIENTED_EDGE ( 'NONE', *, *, #16163, .F. ) ;
#4868 = DIRECTION ( 'NONE',  ( 1.000000000000000000, 0.000000000000000000, 0.000000000000000000 ) ) ;
#4869 = CARTESIAN_POINT ( 'NONE',  ( -48.68588794268870146, 306.9323905601785327, -3.978247347593158345 ) ) ;
#4870 = CARTESIAN_POINT ( 'NONE',  ( 51.93385628276429600, 30.52886280891152282, -94.99999999999994316 ) ) ;
#4871 = CARTESIAN_POINT ( 'NONE',  ( -44.16309181155856578, 335.9948905683720000, 6.410867750099241924 ) ) ;
#4872 = VECTOR ( 'NONE', #4799, 1000.000000000000000 ) ;
#4873 = CARTESIAN_POINT ( 'NONE',  ( -45.64106924314020119, 492.9323905765655809, 11.32908994701042715 ) ) ;
#4874 = CARTESIAN_POINT ( 'NONE',  ( -19.19641293061498644, 370.4323905683720000, -14.20200298773971603 ) ) ;
#4875 = CARTESIAN_POINT ( 'NONE',  ( -47.16347859291443712, 311.3698905765656377, -7.653668647301793193 ) ) ;
#4876 = CARTESIAN_POINT ( 'NONE',  ( -19.19641293061498644, 380.4323905683720568, -14.20200298773971603 ) ) ;
#4877 = CARTESIAN_POINT ( 'NONE',  ( -47.16347859291443712, 321.3698905765656377, -7.653668647301793193 ) ) ;
#4878 = CARTESIAN_POINT ( 'NONE',  ( -174.5421710038924061, 585.7448905601785327, 96.70028278950401557 ) ) ;
#4879 = CARTESIAN_POINT ( 'NONE',  ( -44.16309181155855867, 284.4948905683720000, 6.410867750099241924 ) ) ;
#4880 = CARTESIAN_POINT ( 'NONE',  ( 91.21585410611801592, 31.85652257517428865, 40.00000000000000000 ) ) ;
#4881 = CARTESIAN_POINT ( 'NONE',  ( -25.35362745456399836, 432.5573905683719431, -16.75240474999999307 ) ) ;
#4882 = CARTESIAN_POINT ( 'NONE',  ( -33.45347746554494961, 53.84009227044784041, 120.4403519833905136 ) ) ;
#4883 = LINE ( 'NONE', #9846, #14902 ) ;
#4884 = CARTESIAN_POINT ( 'NONE',  ( -28.68588794268874054, 573.2448905601785327, 0.000000000000000000 ) ) ;
#4885 = CARTESIAN_POINT ( 'NONE',  ( 170.2047888904039610, 610.7448905601785327, -1.893624729818132124 ) ) ;
#4886 = CARTESIAN_POINT ( 'NONE',  ( -28.68588794268871567, 352.8698905683720568, -16.75240474999999307 ) ) ;
#4887 = CARTESIAN_POINT ( 'NONE',  ( -14.48388495494901562, 489.8073905683720568, -9.489475012073736337 ) ) ;
#4888 = VECTOR ( 'NONE', #13183, 1000.000000000000114 ) ;
#4889 = ORIENTED_EDGE ( 'NONE', *, *, #14840, .T. ) ;
#4890 = CARTESIAN_POINT ( 'NONE',  ( -32.66413529028189089, 489.4323905601784759, 19.99999999999999289 ) ) ;
#4891 = CARTESIAN_POINT ( 'NONE',  ( -14.48388495494899431, 309.8073905683720568, -9.489475012073736337 ) ) ;
#4892 = ORIENTED_EDGE ( 'NONE', *, *, #1104, .F. ) ;
#4893 = CARTESIAN_POINT ( 'NONE',  ( -21.03221929538694468, 524.1198905601785327, -18.47759065022572855 ) ) ;
#4894 = ORIENTED_EDGE ( 'NONE', *, *, #19094, .T. ) ;
#4895 = CARTESIAN_POINT ( 'NONE',  ( -33.84809828339280102, 56.85652257517428865, -120.3299889578561448 ) ) ;
#4896 =( BOUNDED_CURVE ( )  B_SPLINE_CURVE ( 2, ( #8394, #18351, #15020, #19978, #10125, #15126, #12068, #13285, #13497, #11962, #203, #19870, #16746, #5046, #20190, #15225, #11647 ),
 .UNSPECIFIED., .F., .T. ) 
 B_SPLINE_CURVE_WITH_KNOTS ( ( 3, 2, 2, 2, 2, 2, 2, 2, 3 ),
 ( 0.01562500000000037470, 0.01757812500000033307, 0.01953125000000028796, 0.02148437500000024286, 0.02343750000000020123, 0.02539062500000015959, 0.02734375000000011449, 0.02929687500000006939, 0.03125000000000002776 ),
 .UNSPECIFIED. ) 
 CURVE ( )  GEOMETRIC_REPRESENTATION_ITEM ( )  RATIONAL_B_SPLINE_CURVE ( ( 0.9999999999999963363, 0.9807852804032340943, 1.000000000000000000, 0.9807852804032304306, 1.000000000000000000, 0.9807852804032304306, 1.000000000000000000, 0.9807852804032304306, 1.000000000000000000, 0.9807852804032304306, 1.000000000000000000, 0.9807852804032304306, 1.000000000000000000, 0.9807852804032304306, 1.000000000000000000, 0.9807852804032302085, 1.000000000000000222 ) ) 
 REPRESENTATION_ITEM ( '' )  );
#4897 = CARTESIAN_POINT ( 'NONE',  ( -16.84014894278199392, 401.6198905683720568, -11.84573899990672707 ) ) ;
#4898 = FACE_OUTER_BOUND ( 'NONE', #12108, .T. ) ;
#4899 = CARTESIAN_POINT ( 'NONE',  ( -18.68588794268873698, 323.8848358243226357, 20.00000000000000355 ) ) ;
#4900 = CARTESIAN_POINT ( 'NONE',  ( -13.20868407381886733, 438.2448905683720000, 6.410867750099229490 ) ) ;
#4901 = MANIFOLD_SOLID_BREP ( 'BearingFace', #7260 ) ;
#4902 = CARTESIAN_POINT ( 'NONE',  ( -11.93348319268873148, 449.1823905683720000, -3.332260488124732856 ) ) ;
#4903 = APPLICATION_PROTOCOL_DEFINITION ( 'draft international standard', 'automotive_design', 1998, #15254 ) ;
#4904 = DIRECTION ( 'NONE',  ( 0.000000000000000000, -1.000000000000000000, 0.000000000000000000 ) ) ;
#4905 = CARTESIAN_POINT ( 'NONE',  ( -28.68588794268871922, 379.4948905765656377, -19.99999999999999289 ) ) ;
#4906 = FACE_OUTER_BOUND ( 'NONE', #18380, .T. ) ;
#4907 = CYLINDRICAL_SURFACE ( 'NONE', #12688, 10.00000000000000178 ) ;
#4908 = CARTESIAN_POINT ( 'NONE',  ( 60.03793209889851568, 30.52886280891152282, -131.1729372809869005 ) ) ;
#4909 = DIRECTION ( 'NONE',  ( -0.8090169943749474513, 0.000000000000000000, -0.5877852522924730261 ) ) ;
#4910 = CARTESIAN_POINT ( 'NONE',  ( -13.20868407381887444, 489.7448905683720568, 6.410867750099229490 ) ) ;
#4911 = ADVANCED_FACE ( 'NONE', ( #14771 ), #8577, .T. ) ;
#4912 = CARTESIAN_POINT ( 'NONE',  ( -28.68588794268874054, 573.2448905601785327, 0.000000000000000000 ) ) ;
#4913 = CARTESIAN_POINT ( 'NONE',  ( -45.64106924314020119, 518.1823905601785327, 11.32908994701042538 ) ) ;
#4914 = B_SPLINE_CURVE_WITH_KNOTS ( 'NONE', 3,
 ( #3429, #10009, #15015, #9756, #11170, #6508, #6729, #6298, #9970, #13126, #6616, #16380, #13013, #19711 ),
 .UNSPECIFIED., .F., .F.,
 ( 4, 2, 2, 2, 2, 2, 4 ),
 ( 0.000000000000000000, 0.002830465529762977734, 0.004245698294644466818, 0.005660931059525955468, 0.007076163824407444118, 0.008491396589288933636, 0.01132186211905188838 ),
 .UNSPECIFIED. ) ;
#4915 = CARTESIAN_POINT ( 'NONE',  ( -32.01814843081345430, 413.1823905683719431, -16.75240474999999307 ) ) ;
#4916 = CARTESIAN_POINT ( 'NONE',  ( -8.685887942688724550, 372.2448905601784759, -2.449293598294705724E-15 ) ) ;
#4917 = ADVANCED_FACE ( 'NONE', ( #18527 ), #12480, .T. ) ;
#4918 = AXIS2_PLACEMENT_3D ( 'NONE', #7079, #14905, #413 ) ;
#4919 = CARTESIAN_POINT ( 'NONE',  ( -38.17536295476244135, 233.8073905683720284, -14.20200298773971426 ) ) ;
#4920 = VERTEX_POINT ( 'NONE', #20370 ) ;
#4921 = CARTESIAN_POINT ( 'NONE',  ( 77.07016797226398808, 161.6844911138030056, -40.00000000000000000 ) ) ;
#4922 = ORIENTED_EDGE ( 'NONE', *, *, #19987, .F. ) ;
#4923 = CARTESIAN_POINT ( 'NONE',  ( -16.84014894278200103, 451.6198905683720568, -11.84573899990672707 ) ) ;
#4924 = CARTESIAN_POINT ( 'NONE',  ( -32.01814843081346851, 531.6823905683719431, -16.75240474999999307 ) ) ;
#4925 = VERTEX_POINT ( 'NONE', #10622 ) ;
#4926 = EDGE_CURVE ( 'NONE', #13370, #10360, #12699, .T. ) ;
#4927 = CARTESIAN_POINT ( 'NONE',  ( -43.60132883224873268, 209.8855831874335820, 1.619299207070719726 ) ) ;
#4928 = CARTESIAN_POINT ( 'NONE',  ( -40.53162694259542320, 222.6198905683720000, -11.84573899990672707 ) ) ;
#4929 = VERTEX_POINT ( 'NONE', #5438 ) ;
#4930 = CARTESIAN_POINT ( 'NONE',  ( -22.27502019258950128, 510.7448905683720000, -15.47720386886985544 ) ) ;
#4931 = FACE_OUTER_BOUND ( 'NONE', #4605, .T. ) ;
#4932 = CARTESIAN_POINT ( 'NONE',  ( -8.685887942688729879, 436.6823905765656377, 3.978247347593161010 ) ) ;
#4933 = DIRECTION ( 'NONE',  ( -1.191790137725560488E-16, 1.000000000000000000, 0.000000000000000000 ) ) ;
#4934 = CARTESIAN_POINT ( 'NONE',  ( -48.68588794268870146, 327.5573905601784759, 3.978247347593168559 ) ) ;
#4935 = CARTESIAN_POINT ( 'NONE',  ( 81.24038404635965094, 30.52886280891152282, 131.1729372809869005 ) ) ;
#4936 = CARTESIAN_POINT ( 'NONE',  ( 125.7989814974898053, 10.52886280891152104, 40.00000000000000000 ) ) ;
#4937 = AXIS2_PLACEMENT_3D ( 'NONE', #14083, #17425, #2501 ) ;
#4938 = EDGE_CURVE ( 'NONE', #15214, #6373, #3818, .T. ) ;
#4939 =( NAMED_UNIT ( * ) PLANE_ANGLE_UNIT ( ) SI_UNIT ( $, .RADIAN. ) );
#4940 = CARTESIAN_POINT ( 'NONE',  ( -48.68588794268872277, 491.9948905765656377, 0.000000000000000000 ) ) ;
#4941 = CARTESIAN_POINT ( 'NONE',  ( -40.53162694259543031, 314.1198905683720568, -11.84573899990672707 ) ) ;
#4942 = CARTESIAN_POINT ( 'NONE',  ( -45.64106924314016567, 236.3073905601784759, -11.32908994701042538 ) ) ;
#4943 = CARTESIAN_POINT ( 'NONE',  ( -32.66413529028186247, 269.4323905601785327, 19.99999999999999289 ) ) ;
#4944 = CARTESIAN_POINT ( 'NONE',  ( -15.54750367907772635, 45.31613216062294214, -120.2864949470673110 ) ) ;
#4945 = CARTESIAN_POINT ( 'NONE',  ( -16.84014894278197971, 281.6198905683720000, -11.84573899990672707 ) ) ;
#4946 = VECTOR ( 'NONE', #13315, 1000.000000000000000 ) ;
#4947 = CARTESIAN_POINT ( 'NONE',  ( -32.01814843081345430, 503.1823905683721136, -16.75240474999999307 ) ) ;
#4948 = VECTOR ( 'NONE', #18651, 1000.000000000000000 ) ;
#4949 = CARTESIAN_POINT ( 'NONE',  ( -24.70764059509556176, 364.4323905601784759, -19.99999999999999289 ) ) ;
#4950 = ADVANCED_FACE ( 'NONE', ( #17341 ), #7479, .F. ) ;
#4951 = ORIENTED_EDGE ( 'NONE', *, *, #6962, .T. ) ;
#4952 = CARTESIAN_POINT ( 'NONE',  ( -45.43829269268871940, 485.0573905683720568, -3.332260488124726194 ) ) ;
#4953 =( NAMED_UNIT ( * ) SI_UNIT ( $, .STERADIAN. ) SOLID_ANGLE_UNIT ( ) );
#4954 = CARTESIAN_POINT ( 'NONE',  ( -16.84014894278197971, 280.1198905683720000, -11.84573899990672707 ) ) ;
#4955 = ORIENTED_EDGE ( 'NONE', *, *, #18846, .T. ) ;
#4956 = DIRECTION ( 'NONE',  ( 0.000000000000000000, 0.000000000000000000, 1.000000000000000000 ) ) ;
#4957 = CARTESIAN_POINT ( 'NONE',  ( -45.43829269268870519, 285.3698905683720568, 0.000000000000000000 ) ) ;
#4958 = EDGE_CURVE ( 'NONE', #8381, #2116, #17997, .T. ) ;
#4959 = AXIS2_PLACEMENT_3D ( 'NONE', #13611, #8720, #15133 ) ;
#4960 = CARTESIAN_POINT ( 'NONE',  ( -21.03221929538690915, 248.8698905765656093, -18.47759065022572855 ) ) ;
#4961 = CARTESIAN_POINT ( 'NONE',  ( -73.08746600497821078, 600.7448905601785327, -22.98912494155474207 ) ) ;
#4962 = LINE ( 'NONE', #2818, #8189 ) ;
#4963 = CARTESIAN_POINT ( 'NONE',  ( -13.20868407381884957, 269.4948905683720000, -6.410867750099233042 ) ) ;
#4964 = VECTOR ( 'NONE', #19570, 1000.000000000000000 ) ;
#4965 = CARTESIAN_POINT ( 'NONE',  ( -40.53162694259543741, 386.6198905683720568, 11.84573899990672885 ) ) ;
#4966 = CARTESIAN_POINT ( 'NONE',  ( -28.68588794268872988, -129.7637193493918915, -49.60091809715359545 ) ) ;
#4967 = CARTESIAN_POINT ( 'NONE',  ( -8.685887942688733432, 456.9948905765656377, -2.449293598294705724E-15 ) ) ;
#4968 = CARTESIAN_POINT ( 'NONE',  ( -47.16347859291443712, 271.3698905765656377, -7.653668647301793193 ) ) ;
#4969 = CARTESIAN_POINT ( 'NONE',  ( -45.43829269268871940, 423.8698905683720568, 0.000000000000000000 ) ) ;
#4970 = CARTESIAN_POINT ( 'NONE',  ( 166.1493775951145437, 620.7448905601785327, 8.917803138848105604 ) ) ;
#4971 = ORIENTED_EDGE ( 'NONE', *, *, #14181, .T. ) ;
#4972 = CARTESIAN_POINT ( 'NONE',  ( -8.685887942688728103, 422.2448905601784759, -2.449293598294705724E-15 ) ) ;
#4973 = ORIENTED_EDGE ( 'NONE', *, *, #2754, .F. ) ;
#4974 = ORIENTED_EDGE ( 'NONE', *, *, #4522, .T. ) ;
#4975 = ORIENTED_EDGE ( 'NONE', *, *, #5721, .F. ) ;
#4976 = CARTESIAN_POINT ( 'NONE',  ( -8.685887942688715668, 302.5573905601784759, -3.978247347593165895 ) ) ;
#4977 = FACE_OUTER_BOUND ( 'NONE', #1089, .T. ) ;
#4978 = CARTESIAN_POINT ( 'NONE',  ( -22.27502019258948707, 352.2448905683720000, -15.47720386886985544 ) ) ;
#4979 = ORIENTED_EDGE ( 'NONE', *, *, #9999, .T. ) ;
#4980 = CARTESIAN_POINT ( 'NONE',  ( -11.73070664223726567, 487.9323905765656377, -11.32908994701042715 ) ) ;
#4981 = CARTESIAN_POINT ( 'NONE',  ( -42.88789093042843348, 362.9323905683720568, -9.489475012073736337 ) ) ;
#4982 = CARTESIAN_POINT ( 'NONE',  ( 62.02695467647412642, 160.1716627696692399, -61.71700053422263466 ) ) ;
#4983 = CARTESIAN_POINT ( 'NONE',  ( -11.93348319268872260, 379.1823905683721136, -3.332260488124732856 ) ) ;
#4984 = CARTESIAN_POINT ( 'NONE',  ( -40.01497788969913216, 300.4323905765656377, -16.95518130045146421 ) ) ;
#4985 = CARTESIAN_POINT ( 'NONE',  ( 40.42502041961814996, 180.1716627696692967, -20.00000000000000355 ) ) ;
#4986 = CARTESIAN_POINT ( 'NONE',  ( -35.09675569278794427, 285.7448905683720568, 15.47720386886985366 ) ) ;
#4987 = LINE ( 'NONE', #18393, #21195 ) ;
#4988 = ADVANCED_FACE ( 'NONE', ( #5654 ), #12475, .T. ) ;
#4989 = CARTESIAN_POINT ( 'NONE',  ( -45.43829269268871940, 435.3698905683720000, 0.000000000000000000 ) ) ;
#4990 = EDGE_CURVE ( 'NONE', #15032, #14472, #17028, .T. ) ;
#4991 = LINE ( 'NONE', #6495, #6813 ) ;
#4992 = CARTESIAN_POINT ( 'NONE',  ( -24.70764059509556532, 500.0573905601785896, 19.99999999999998934 ) ) ;
#4993 = LINE ( 'NONE', #3056, #9879 ) ;
#4994 = CARTESIAN_POINT ( 'NONE',  ( 35.96497763894178945, 230.5765313837437418, -60.00000000000000000 ) ) ;
#4995 = CARTESIAN_POINT ( 'NONE',  ( -22.27502019258947641, 348.4948905683720000, 15.47720386886985189 ) ) ;
#4996 = CARTESIAN_POINT ( 'NONE',  ( -40.53162694259545162, 475.1198905683720000, 11.84573899990672885 ) ) ;
#4997 = ORIENTED_EDGE ( 'NONE', *, *, #19579, .F. ) ;
#4998 = CARTESIAN_POINT ( 'NONE',  ( -17.35679799567830628, 480.6823905601784759, 16.95518130045146421 ) ) ;
#4999 = CARTESIAN_POINT ( 'NONE',  ( -28.68588794268870501, 306.3698905683720568, 16.75240474999999307 ) ) ;
#5000 = ORIENTED_EDGE ( 'NONE', *, *, #17107, .T. ) ;
#5001 = DIRECTION ( 'NONE',  ( -0.000000000000000000, 0.000000000000000000, -1.000000000000000000 ) ) ;
#5002 = ORIENTED_EDGE ( 'NONE', *, *, #11425, .T. ) ;
#5003 = FACE_OUTER_BOUND ( 'NONE', #14285, .T. ) ;
#5004 = CARTESIAN_POINT ( 'NONE',  ( -45.43829269268871940, 395.3698905683720000, 0.000000000000000000 ) ) ;
#5005 = CARTESIAN_POINT ( 'NONE',  ( 51.98438129372387806, 30.52886280891151216, 117.7249735956185219 ) ) ;
#5006 = CARTESIAN_POINT ( 'NONE',  ( -11.73070664223724968, 386.0573905765656946, 11.32908994701042005 ) ) ;
#5007 = CARTESIAN_POINT ( 'NONE',  ( -32.01814843081345430, 431.6823905683720000, -16.75240474999999307 ) ) ;
#5008 = CARTESIAN_POINT ( 'NONE',  ( -44.16309181155857999, 454.4948905683720568, 6.410867750099241924 ) ) ;
#5009 =( NAMED_UNIT ( * ) PLANE_ANGLE_UNIT ( ) SI_UNIT ( $, .RADIAN. ) );
#5010 = CARTESIAN_POINT ( 'NONE',  ( 52.60622592008805043, 10.52886280891152104, -151.0302712373927250 ) ) ;
#5011 = CARTESIAN_POINT ( 'NONE',  ( -10.20829729246298712, 366.3698905765655809, 7.653668647301790529 ) ) ;
#5012 = CARTESIAN_POINT ( 'NONE',  ( -18.70553453894068952, 45.88067589482868414, 48.58894481687972444 ) ) ;
#5013 = CARTESIAN_POINT ( 'NONE',  ( -40.01497788969912506, 265.6823905601785327, -16.95518130045146421 ) ) ;
#5014 = CARTESIAN_POINT ( 'NONE',  ( -8.685887942688731655, 548.2448905601784190, 0.000000000000000000 ) ) ;
#5015 = LINE ( 'NONE', #10195, #18664 ) ;
#5016 = CARTESIAN_POINT ( 'NONE',  ( -35.09675569278796559, 497.2448905683720000, 15.47720386886985366 ) ) ;
#5017 = CARTESIAN_POINT ( 'NONE',  ( 20.74841189052421697, 600.7448905601785327, 7.500000000000000000 ) ) ;
#5018 = CARTESIAN_POINT ( 'NONE',  ( -48.68588794268857356, 466.9323905601784759, -3.978247347593530936 ) ) ;
#5019 = CARTESIAN_POINT ( 'NONE',  ( -43.37443857369948574, 209.1166545091122657, 3.053198389463522844 ) ) ;
#5020 = CARTESIAN_POINT ( 'NONE',  ( -19.19641293061498644, 398.8073905683720568, 14.20200298773971426 ) ) ;
#5021 = CARTESIAN_POINT ( 'NONE',  ( 1.336753550880579347E-14, 213.9102039777116602, 33.59072564020503648 ) ) ;
#5022 =( BOUNDED_SURFACE ( )  B_SPLINE_SURFACE ( 1, 2, ( 
 ( #13475, #9991, #75, #19849, #15208, #8585, #6642, #10206, #18436, #15318, #8374, #13586, #7065, #20068, #5447, #288, #2219, #18637, #13684, #3724, #183, #2017, #16829, #5137, #10308, #13263, #503, #397, #16933, #14997, #2115, #3623, #6964, #5026, #19959, #8694, #20277, #10103, #12048, #3828, #1805, #18221, #20175, #5341, #11627, #3414, #16725, #11736, #18326, #16615, #10416, #6751, #5240, #11942, #13369, #17037, #14888, #3516, #1913, #8481, #15104, #6857, #11840, #2325, #18851, #2639, #819, #4143, #17247, #12372, #17351, #2534, #707, #10848, #5763, #15524, #4040, #5553, #9117, #9011, #15844, #603, #9226, #10738, #7490, #7386, #12159, #7278, #13901, #10950, #19078, #15738, #15418, #20491, #10629, #5662, #926, #5984, #12267, #18747, #8904, #7595, #3935, #20592, #2430, #13791, #20812, #8801, #15634, #12593, #10521, #12485, #7168, #14012, #17143, #4260, #1031, #20380, #14226, #18962, #14115, #20701, #5874, #17452, #19186, #4364, #17560, #6757, #82, #5453, #5246, #15213, #16622, #17045, #8487, #1812, #13375, #16732, #6863, #18333, #8380, #11846, #8590, #13269, #6969, #3420, #7071, #18443, #404, #5144, #18542, #12055, #9998, #15004, #19855, #10110, #16834, #3629, #3523, #190, #1919, #10423, #11742, #15110, #13691, #13482, #19965, #15323, #294, #2226, #8807, #20075, #10211, #6648, #5032, #2022, #18643, #11633, #13592, #20179, #5347, #11948, #3729, #16938, #10314, #2120, #18228, #8701, #508, #20283, #3835, #17458, #7285, #609, #932, #9123, #2758, #2647, #3942, #13908, #10744, #20598, #12378, #4267, #10527, #14232, #4152, #10854, #14019, #17254, #17358, #15532, #20498, #9233, #18971, #713, #10636, #12166, #15745, #15640, #1037, #7174, #15853, #2540, #12494, #18857, #5990, #2330, #19084, #7601, #12600, #13796, #20387, #826, #7498, #19192, #14121, #5668, #20820, #5561, #20708, #8911, #4371, #2437, #12276, #5881, #10957, #17566, #15424, #18754, #4047, #17149, #9018, #7392, #5771, #4787, #14545, #6196, #4684, #6304, #1452, #7713, #9447, #19400, #3181, #17877, #19294, #13130, #7917, #4480, #15956, #14342, #9654, #3070, #1142, #11279, #12916, #9760, #2864, #8025, #1559, #21131, #21346, #16168, #18094, #19717, #8129, #13018, #16065, #16275, #14658, #21026, #19610, #20922, #16384, #21239, #11384, #1241, #17982, #19506, #6405, #6089, #14446, #14761, #6514, #4583, #4900, #11497, #17670, #12703, #9335, #11063, #7815, #12808, #11175, #17777, #2970, #9548, #1344, #19832, #15084, #18413, #9863, #372, #20043, #6836, #13242, #5007, #3703, #3289, #16703, #18198, #13348, #18517, #1892, #5220, #11714, #13452, #11819, #3602, #10186, #6942, #6733, #15297, #11607, #13566, #20154, #484, #16489, #1671, #10082, #16807, #7048, #1997, #14975, #5322, #8240, #8566, #3395, #2092, #18306, #8351, #15187, #11923, #10291, #8673, #16912, #19936, #13668, #6621, #9975, #5428, #20257, #8459, #162, #12028, #269, #14871, #50, #16594, #5114, #1783, #3495, #7151, #1013, #17230, #13772, #3807, #2199, #18942, #12355, #10398, #13994, #801, #19061, #12141, #17333, #10828, #2413, #9203, #4019, #5962, #7579, #17438, #905, #3915, #5744, #20576, #8888, #7470, #17017, #4243, #4127, #14100, #18727, #20681, #7367, #10715, #8784, #2305, #5856, #12463, #13883, #2622, #15829, #5536, #583, #2516, #9100, #15400, #20361, #20474, #15505, #690, #10505, #14206, #17126, #8993, #15721, #7258, #20795, #18620, #5643, #12251, #18834, #10612, #15614, #4561, #6066, #1220, #6381, #11148, #7893, #21004, #16141, #21106, #6278, #4451, #14631, #9523, #19271, #7790, #9312, #12892, #12782, #19583, #4348, #12990, #15929, #12677, #11358, #7689, #2944, #11037, #17541, #3155, #12576, #19376, #16356, #1118, #16248, #10931, #17753, #14319, #7999, #4763, #2732, #17955, #14423, #20898, #1322, #17648, #2840, #9422, #19170, #9734, #16042, #6172, #1533, #14521, #19482, #4662, #8103, #11253, #17852, #3046, #9629, #1427, #21216, #14733, #21315, #15058, #19688, #13427, #9837, #13539, #11689, #241, #11580, #3576, #18491, #16460, #1643, #4874, #16568, #1865, #18280, #9948, #8215, #1754, #16884, #18171, #8326, #20128, #13324, #19, #350, #14843, #2068, #8643, #3369, #13216, #15271, #13103, #6595, #11898, #11468, #4981, #14948, #134, #6707, #19801, #1968, #20018, #5194, #6486, #19907, #15162, #11791, #18066, #8540, #5088, #3261, #18387, #6811, #3468, #6913, #10055, #16678, #8436, #10165, #16783, #5295, #3680, #10264, #10581, #17307, #20444, #2278, #17204, #555, #20553, #13853, #18594, #20336, #13750, #2598, #10688, #2383, #7020, #5508, #10477, #12109, #8966, #19033, #7124, #5617, #8858, #15590, #18702, #5719, #12225, #3779, #3888, #17099, #9178, #2492, #773, #13643, #15479, #664, #7230, #7337, #4218, #18808, #10369, #15377, #20656, #16994, #3990, #13970, #5399, #12436, #455, #12327, #10801, #2172, #4100, #20229, #18915, #8757, #9073, #15694, #12004, #14071, #881, #7445, #5826, #17416, #20770, #1096, #990, #7977, #7664, #15803, #21187, #20979, #9502, #10906, #11336, #2814, #17517, #14292, #11013, #1198, #12652, #2708, #6147, #2922, #7554, #1294, #19146, #1401, #12759, #16116, #20878, #12865, #6358, #4323, #9289, #14179, #4429, #11122, #19348, #19246, #15905, #17622, #4739, #6043, #9397, #14604, #7769, #16016, #9605, #14395, #17931, #3127, #4536, #17727, #5937, #12552, #7870, #12968, #14499, #21082, #6254, #19455, #4638, #11232, #17829, #3023, #16224, #19559, #1507, #4842, #13077, #9712, #11441, #8082, #16332, #18041, #14712, #21289, #6461, #19664, #576, #4013, #13879, #5639, #18938, #3802, #7465, #18830, #4121, #10394, #11119, #10709, #20469, #5531, #10607, #12247, #797, #7044, #8779, #18723, #2512, #17225, #18616, #12456, #7252, #17013, #15293, #13663, #8988, #2407, #480, #15610, #7362, #9097, #2195, #13990, #901, #20572, #20676, #15500, #17722, #19056, #14095, #12349, #15396, #5739, #17329, #20356, #15716, #20251, #5851, #4239, #8669, #7145, #5423, #12024, #13769, #12136, #3911, #10501, #17121, #2300, #8882, #685, #11229, #6251, #1611, #11438, #16112, #1290, #4736, #14601, #7972, #19452, #16538, #4635, #14708, #18038, #9499, #10383, #19658, #6458, #12862, #17826, #3337, #2919, #16328, #3019, #12965, #18142, #1504, #4838, #11332, #13074, #3233, #9810, #16220, #4954, #21285, #9602, #19555, #21077, #16433, #3124, #9919, #7867, #1723, #8184, #6563, #6355, #14920, #1397, #13184, #19768, #103, #14496, #21184, #9708, #14814, #6676, #11553, #17927, #8295, #8079, #13295, #19880, #5057, #11660, #1944, #6995, #8725, #11974, #17071, #10450, #320, #634, #215, #16653, #2253, #13508, #1835, #2043, #8407, #15031, #3550, #3443, #8830, #10137, #18251, #15451, #8614, #18571, #13402, #13823, #5270, #19989, #16757, #20101, #3654, #15139, #5169, #15239, #5369, #10027, #3753, #6782, #3860, #429, #10341, #8512, #15352, #7200, #11765, #18360, #6889, #11875, #13617, #20204, #18465, #10236, #16861, #20416, #16965, #2145, #5588, #533, #7098, #12080, #13717, #20310, #5480, #18671, #18888, #1167, #18781, #15560, #17592, #10555, #10660, #20625, #9044, #15666, #7310, #7635, #19113, #4295, #14369, #12299, #20846, #10879, #17177, #14260, #4074, #3965, #17484, #5909, #20948, #6017, #745, #17278, #7524, #17385, #9148, #1065, #13937, #10983, #960, #12626, #10770, #14043, #14149, #2464, #2674, #4183, #8935, #852, #7417, #12193, #19217, #20736, #2357, #5800, #12406, #18998, #12519, #15986, #2568, #20527, #5692, #2784, #15770, #9260, #15877, #4400, #7740, #6120, #6331, #9892, #9475, #9784, #19319, #11306, #16086, #1586, #21371, #18117, #14471, #16408, #8156, #3313, #4505, #11094, #12944, #21262, #16515, #6429, #17803, #14786, #17698, #16304, #21052, #4928, #14574, #11204, #1476, #18013, #13045, #11525, #19744, #9577 ),
 ( #1265, #6539, #2892, #17902, #7842, #13156, #1696, #6222, #8265, #1372, #12837, #3097, #19426, #4611, #2993, #16193, #14896, #7942, #21158, #19531, #9680, #19634, #4709, #8053, #14685, #4814, #11408, #3206, #12306, #2365, #7208, #17287, #14051, #18680, #12415, #8838, #12528, #10669, #20635, #10562, #2579, #17495, #15459, #642, #3867, #15567, #860, #2471, #8944, #13830, #753, #16177, #17185, #7318, #19123, #18896, #20424, #20745, #5597, #1354, #7927, #13946, #12201, #14556, #12088, #18788, #10888, #10457, #3972, #20533, #5700, #4082, #9052, #969, #19010, #15675, #5919, #5808, #7424, #9270, #4193, #10779, #17077, #17396, #9158, #15782, #7533, #14159, #4305, #2685, #5488, #19841, #13358, #19727, #11724, #6521, #8470, #3506, #19947, #3403, #6413, #8250, #16497, #11392, #9983, #6314, #6742, #14879, #16605, #21248, #1794, #9872, #62, #12928, #4796, #8362, #14985, #16394, #172, #5124, #8037, #3079, #5016, #6631, #19515, #4694, #1568, #17993, #3190, #16286, #18316, #1462, #11506, #13251, #11288, #18207, #1679, #3299, #9662, #14668, #10092, #21143, #13138, #13027, #9768, #16713, #4910, #11616, #8138, #1903, #17886, #19619, #14769, #21355, #18104, #383, #10298, #11830, #591, #15305, #697, #6847, #8895, #17025, #12148, #18525, #5651, #2007, #18737, #10511, #12257, #13462, #279, #491, #8791, #18840, #7158, #5331, #3921, #20055, #3815, #8575, #13890, #2103, #20164, #10407, #5542, #13780, #20480, #7266, #3711, #4028, #18424, #15198, #17236, #17133, #20264, #11932, #2205, #12036, #20368, #5231, #6953, #18627, #2314, #10196, #10620, #15513, #2420, #13674, #16922, #15094, #13576, #3611, #7056, #8681, #5435, #915, #11156, #19277, #4354, #15621, #7477, #19068, #14106, #10938, #6179, #15728, #5752, #2524, #7797, #4133, #20801, #20690, #14003, #21011, #9000, #9213, #12789, #12362, #12684, #809, #14214, #18952, #4460, #2846, #7375, #1226, #4250, #20582, #5971, #10725, #17339, #5864, #9107, #14430, #12472, #10837, #19382, #12582, #2739, #17443, #4567, #2630, #15834, #1021, #7585, #19176, #17549, #9320, #15937, #1125, #7696, #14325, #20905, #16048, #6072, #11044, #17654, #9430, #17760, #6285, #12899, #16148, #12999, #19695, #14742, #6388, #19489, #19591, #13332, #14639, #4770, #9954, #9741, #17859, #18179, #4669, #19914, #5095, #21224, #9637, #11696, #9530, #11260, #8332, #1328, #1435, #11365, #17961, #3163, #3053, #19812, #9844, #16468, #2951, #16257, #11587, #1651, #7900, #4989, #8005, #14528, #8223, #18074, #21113, #3377, #16362, #1540, #4881, #8111, #21326, #6494, #14955, #13111, #11477, #6715, #3269, #6602, #14852, #27, #13224, #16576, #1763, #141, #10484, #13545, #16685, #2074, #8442, #1872, #3582, #3476, #17105, #10170, #18288, #2285, #8652, #12011, #13433, #13863, #5303, #20026, #16790, #20136, #3686, #15168, #5201, #15279, #5406, #10062, #3787, #249, #3896, #462, #18603, #1977, #15384, #8865, #6818, #11798, #15066, #6921, #13650, #7028, #357, #18395, #11904, #7236, #8548, #18497, #15485, #10273, #16892, #12119, #20235, #20451, #5623, #10378, #17000, #2180, #8764, #563, #670, #7130, #13757, #20342, #5517, #18708, #7344, #7672, #19154, #4329, #14402, #12334, #20882, #10911, #10589, #14299, #4106, #18815, #17523, #5943, #20983, #6049, #782, #10695, #7559, #17422, #9185, #1101, #13977, #11017, #996, #12657, #10808, #14079, #14186, #18922, #2714, #4226, #8972, #17315, #2498, #12233, #19251, #20778, #3996, #9081, #888, #15701, #12560, #9403, #7451, #15597, #5726, #17627, #20559, #2604, #20662, #17210, #2390, #9295, #15909, #5833, #4434, #15810, #2819, #12442, #16022, #1203, #7773, #19041, #12973, #14932, #9928, #4965, #9818, #12872, #14716, #1513, #17834, #16442, #12764, #13197, #21294, #1621, #6259, #8195, #16338, #6466, #19353, #11236, #14823, #2, #1406, #6575, #19778, #14504, #9506, #4849, #13083, #4543, #11127, #7983, #3029, #9612, #1302, #11563, #7874, #17937, #19669, #17733, #3243, #8086, #9718, #16121, #21086, #18150, #6151, #19563, #19462, #16229, #3348, #4744, #11447, #14611, #18048, #16548, #1733, #4645, #8307, #3132, #21196, #6363, #2926, #11342, #330, #7109, #13306, #15362, #2052, #18579, #3560, #12092, #8418, #3765, #16975, #18683, #19891, #6688, #6897, #15250, #3872, #436, #11774, #10352, #5067, #10245, #15041, #20319, #8522, #5177, #16870, #11985, #7003, #5491, #13729, #10150, #10460, #3452, #1848, #2263, #2157, #5279, #18371, #8626, #18475, #13627, #11671, #225, #16766, #542, #20214, #10037, #17081, #20110, #8737, #18261, #8841, #5379, #114, #6792, #16663, #13410, #19999, #1953, #15148, #13519, #11884, #3662, #17498, #1077, #2368, #18793, #14163, #2583, #7211, #13833, #17289, #5703, #20537, #10565, #7648, #17188, #5811, #9161, #645, #12532, #10783, #19013, #3975, #8947, #15889, #15462, #7427, #15570, #4085, #9273, #14054, #17399, #2474, #4196, #15785, #972, #7322, #2688, #12419, #756, #10672, #12204, #7536, #15678, #14275, #20427, #20858, #20748, #19126, #18899, #6028, #13949, #4308, #10891, #12638, #5600, #12309, #864, #5922, #19230, #4413, #9057, #10996, #20638, #17605, #2796, #8172, #17816, #14484, #19544, #21273, #3112, #14802, #1598, #12848, #13171, #12741, #11106, #11540, #4827, #14588, #6236, #4724, #6343, #1491, #7751, #9488, #19439, #3220, #17915, #19332, #19757, #7958, #4518, #16000, #14380, #9695, #16316, #1181, #11320, #12955, #9798, #2905, #8066, #21386, #21172, #6552, #16207, #18131, #4941, #9382, #13061, #16098, #14696, #6444, #21064, #20962, #17710, #1277, #6133, #11424, #19647, #4622, #18026, #16420, #7855, #11217, #3006, #9591, #1385, #11859, #13284, #7083, #1932, #19869, #9906, #8279, #3642, #18454, #16527, #20089, #6876, #3740, #18240, #2033, #16950, #8499, #15338, #10124, #12067, #13704, #2132, #6983, #10013, #10223, #5259, #15018, #13603, #1711, #10328, #16848, #20189, #3432, #5358, #13496, #8601, #14910, #8393, #11960, #18557, #19977, #8713, #521, #11646, #6663, #15224, #417, #93, #5045, #5157, #202, #6769, #16638, #20297, #1823, #15125, #5467, #13390, #3324, #11753, #18349, #3536, #16745, #307, #18657, #12288, #5576, #15547, #9136, #5681, #2451, #7298, #10646, #15655, #841, #18767, #17373, #17266, #12181, #729, #15436, #7405, #13924, #945, #10437, #15757, #9029, #12391, #8923, #20721, #20401, #18985, #2555, #5896, #17058, #3849, #18872, #20611, #4282, #5787, #20512, #7512, #8819, #14031, #3955, #12506, #4062, #4166, #10758, #14135, #19099, #2241, #624, #7187, #2343, #13810, #10542, #17162, #13669, #11924, #20155, #5115, #18307, #17018, #16595, #8567, #10083, #5221, #10399, #15188, #18518, #3603, #5323, #3704, #10292, #8460, #18621, #13567, #1893, #11820, #13349, #16913, #16808, #2200, #8352, #8785, #2093, #20258, #20044, #7152, #3496, #5429, #12029, #13773, #14976, #1784, #1998, #8674, #20362, #15298, #6837, #3808, #163, #485, #16704, #15401, #10187, #270, #7049, #584, #5537, #12142, #18728, #18414, #3916, #19937, #15085, #6734, #11715, #373, #13453, #6943, #7471, #2623, #8889, #10613, #20577, #4349, #19062, #20475, #14320, #9101, #5644, #17127, #15506, #10829, #4244, #2306, #5857, #14101, #10932, #4020, #9204, #2733, #15722, #1119, #17334, #19272, #20899, #9313, #14207, #17231, #17439, #12464, #802, #20796, #691, #17542, #15830, #5963, #2414, #12577, #20682, #1014, #7259, #15615, #19171, #15930, #5745, #7690, #6067, #18835, #13884, #7580, #12678, #12252, #8994, #12356, #7368, #13995, #18943, #10506, #4128, #10716, #2517, #906, #9630, #1428, #14734, #21005, #3262, #14632, #21316, #3047, #6279, #21217, #4562, #3156, #17853, #1221, #2945, #17754, #6596, #6487, #6382, #11038, #9524, #14522, #16142, #12991, #1644, #11149, #7791, #19377, #9838, #6173 ) ),
 .UNSPECIFIED., .F., .F., .T. ) 
 B_SPLINE_SURFACE_WITH_KNOTS ( ( 2, 2 ),
 ( 3, 2, 2, 2, 2, 2, 2, 2, 2, 2, 2, 2, 2, 2, 2, 2, 2, 2, 2, 2, 2, 2, 2, 2, 2, 2, 2, 2, 2, 2, 2, 2, 2, 2, 2, 2, 2, 2, 2, 2, 2, 2, 2, 2, 2, 2, 2, 2, 2, 2, 2, 2, 2, 2, 2, 2, 2, 2, 2, 2, 2, 2, 2, 2, 2, 2, 2, 2, 2, 2, 2, 2, 2, 2, 2, 2, 2, 2, 2, 2, 2, 2, 2, 2, 2, 2, 2, 2, 2, 2, 2, 2, 2, 2, 2, 2, 2, 2, 2, 2, 2, 2, 2, 2, 2, 2, 2, 2, 2, 2, 2, 2, 2, 2, 2, 2, 2, 2, 2, 2, 2, 2, 2, 2, 2, 2, 2, 2, 2, 2, 2, 2, 2, 2, 2, 2, 2, 2, 2, 2, 2, 2, 2, 2, 2, 2, 2, 2, 2, 2, 2, 2, 2, 2, 2, 2, 2, 2, 2, 2, 2, 2, 2, 2, 2, 2, 2, 2, 2, 2, 2, 2, 2, 2, 2, 2, 2, 2, 2, 2, 2, 2, 2, 2, 2, 2, 2, 2, 2, 2, 2, 2, 2, 2, 2, 2, 2, 2, 2, 2, 2, 2, 2, 2, 2, 2, 2, 2, 2, 2, 2, 2, 2, 2, 2, 2, 2, 2, 2, 2, 2, 2, 2, 2, 2, 2, 2, 2, 2, 2, 2, 2, 2, 2, 2, 2, 2, 2, 2, 2, 2, 2, 2, 2, 2, 2, 2, 2, 2, 2, 2, 2, 2, 2, 2, 2, 2, 2, 2, 2, 2, 2, 2, 2, 2, 2, 2, 2, 2, 2, 2, 2, 2, 2, 2, 2, 2, 2, 2, 2, 2, 2, 2, 2, 2, 2, 2, 2, 2, 2, 2, 2, 2, 2, 2, 2, 2, 2, 2, 2, 2, 2, 2, 2, 2, 2, 2, 2, 2, 2, 2, 2, 2, 2, 2, 2, 2, 2, 2, 2, 2, 2, 2, 2, 2, 2, 2, 2, 2, 2, 2, 2, 2, 2, 2, 2, 2, 2, 2, 2, 2, 2, 2, 2, 2, 2, 2, 2, 2, 2, 2, 2, 2, 2, 2, 2, 2, 2, 2, 2, 2, 2, 2, 2, 2, 2, 2, 2, 2, 2, 2, 2, 2, 2, 2, 2, 2, 2, 2, 2, 2, 2, 2, 2, 2, 2, 2, 2, 2, 2, 2, 2, 2, 2, 2, 2, 2, 2, 2, 2, 2, 2, 2, 2, 2, 2, 2, 2, 2, 2, 2, 2, 2, 2, 2, 2, 2, 2, 2, 2, 2, 2, 2, 2, 2, 2, 2, 2, 2, 2, 2, 2, 2, 2, 2, 2, 2, 2, 2, 2, 2, 2, 2, 2, 2, 2, 2, 2, 2, 2, 2, 2, 2, 2, 2, 2, 2, 2, 2, 2, 2, 2, 2, 2, 2, 2, 2, 2, 2, 2, 2, 2, 2, 2, 2, 2, 2, 2, 2, 2, 2, 2, 2, 2, 2, 2, 2, 2, 2, 2, 2, 2, 2, 2, 2, 2, 2, 2, 2, 2, 2, 2, 3 ),
 ( 0.000000000000000000, 1.000000000000000000 ),
 ( 0.000000000000000000, 0.001953125000000000000, 0.003906250000000000000, 0.005859375000000000000, 0.007812500000000000000, 0.009765625000000000000, 0.01171875000000000000, 0.01367187500000000000, 0.01562500000000000000, 0.01757812500000000000, 0.01953125000000000000, 0.02148437500000000000, 0.02343750000000000000, 0.02539062500000000000, 0.02734375000000000000, 0.02929687500000000000, 0.03125000000000000000, 0.03320312500000000000, 0.03515625000000000000, 0.03710937500000000000, 0.03906250000000000000, 0.04101562500000000000, 0.04296875000000000000, 0.04492187500000000000, 0.04687500000000000000, 0.04882812500000000000, 0.05078125000000000000, 0.05273437500000000000, 0.05468750000000000000, 0.05664062500000000000, 0.05859375000000000000, 0.06054687500000000000, 0.06250000000000000000, 0.06445312500000000000, 0.06640625000000000000, 0.06835937500000000000, 0.07031250000000000000, 0.07226562500000000000, 0.07421875000000000000, 0.07617187500000000000, 0.07812500000000000000, 0.08007812500000000000, 0.08203125000000000000, 0.08398437500000000000, 0.08593750000000000000, 0.08789062500000000000, 0.08984375000000000000, 0.09179687500000000000, 0.09375000000000000000, 0.09570312500000000000, 0.09765625000000000000, 0.09960937500000000000, 0.1015625000000000000, 0.1035156250000000000, 0.1054687500000000000, 0.1074218750000000000, 0.1093750000000000000, 0.1113281250000000000, 0.1132812500000000000, 0.1152343750000000000, 0.1171875000000000000, 0.1191406250000000000, 0.1210937500000000000, 0.1230468750000000000, 0.1250000000000000000, 0.1269531250000000000, 0.1289062500000000000, 0.1308593750000000000, 0.1328125000000000000, 0.1347656250000000000, 0.1367187500000000000, 0.1386718750000000000, 0.1406250000000000000, 0.1425781250000000000, 0.1445312500000000000, 0.1464843750000000000, 0.1484375000000000000, 0.1503906250000000000, 0.1523437500000000000, 0.1542968750000000000, 0.1562500000000000000, 0.1582031250000000000, 0.1601562500000000000, 0.1621093750000000000, 0.1640625000000000000, 0.1660156250000000000, 0.1679687500000000000, 0.1699218750000000000, 0.1718750000000000000, 0.1738281250000000000, 0.1757812500000000000, 0.1777343750000000000, 0.1796875000000000000, 0.1816406250000000000, 0.1835937500000000000, 0.1855468750000000000, 0.1875000000000000000, 0.1894531250000000000, 0.1914062500000000000, 0.1933593750000000000, 0.1953125000000000000, 0.1972656250000000000, 0.1992187500000000000, 0.2011718750000000000, 0.2031250000000000000, 0.2050781250000000000, 0.2070312500000000000, 0.2089843750000000000, 0.2109375000000000000, 0.2128906250000000000, 0.2148437500000000000, 0.2167968750000000000, 0.2187500000000000000, 0.2207031250000000000, 0.2226562500000000000, 0.2246093750000000000, 0.2265625000000000000, 0.2285156250000000000, 0.2304687500000000000, 0.2324218750000000000, 0.2343750000000000000, 0.2363281250000000000, 0.2382812500000000000, 0.2402343750000000000, 0.2421875000000000000, 0.2441406250000000000, 0.2460937500000000000, 0.2480468750000000000, 0.2500000000000000000, 0.2519531250000000000, 0.2539062500000000000, 0.2558593750000000000, 0.2578125000000000000, 0.2597656250000000000, 0.2617187500000000000, 0.2636718750000000000, 0.2656250000000000000, 0.2675781250000000000, 0.2695312500000000000, 0.2714843750000000000, 0.2734375000000000000, 0.2753906250000000000, 0.2773437500000000000, 0.2792968750000000000, 0.2812500000000000000, 0.2832031250000000000, 0.2851562500000000000, 0.2871093750000000000, 0.2890625000000000000, 0.2910156250000000000, 0.2929687500000000000, 0.2949218750000000000, 0.2968750000000000000, 0.2988281250000000000, 0.3007812500000000000, 0.3027343750000000000, 0.3046875000000000000, 0.3066406250000000000, 0.3085937500000000000, 0.3105468750000000000, 0.3125000000000000000, 0.3144531250000000000, 0.3164062500000000000, 0.3183593750000000000, 0.3203125000000000000, 0.3222656250000000000, 0.3242187500000000000, 0.3261718750000000000, 0.3281250000000000000, 0.3300781250000000000, 0.3320312500000000000, 0.3339843750000000000, 0.3359375000000000000, 0.3378906250000000000, 0.3398437500000000000, 0.3417968750000000000, 0.3437500000000000000, 0.3457031250000000000, 0.3476562500000000000, 0.3496093750000000000, 0.3515625000000000000, 0.3535156250000000000, 0.3554687500000000000, 0.3574218750000000000, 0.3593750000000000000, 0.3613281250000000000, 0.3632812500000000000, 0.3652343750000000000, 0.3671875000000000000, 0.3691406250000000000, 0.3710937500000000000, 0.3730468750000000000, 0.3750000000000000000, 0.3769531250000000000, 0.3789062500000000000, 0.3808593750000000000, 0.3828125000000000000, 0.3847656250000000000, 0.3867187500000000000, 0.3886718750000000000, 0.3906250000000000000, 0.3925781250000000000, 0.3945312500000000000, 0.3964843750000000000, 0.3984375000000000000, 0.4003906250000000000, 0.4023437500000000000, 0.4042968750000000000, 0.4062500000000000000, 0.4082031250000000000, 0.4101562500000000000, 0.4121093750000000000, 0.4140625000000000000, 0.4160156250000000000, 0.4179687500000000000, 0.4199218750000000000, 0.4218750000000000000, 0.4238281250000000000, 0.4257812500000000000, 0.4277343750000000000, 0.4296875000000000000, 0.4316406250000000000, 0.4335937500000000000, 0.4355468750000000000, 0.4375000000000000000, 0.4394531250000000000, 0.4414062500000000000, 0.4433593750000000000, 0.4453125000000000000, 0.4472656250000000000, 0.4492187500000000000, 0.4511718750000000000, 0.4531250000000000000, 0.4550781250000000000, 0.4570312500000000000, 0.4589843750000000000, 0.4609375000000000000, 0.4628906250000000000, 0.4648437500000000000, 0.4667968750000000000, 0.4687500000000000000, 0.4707031250000000000, 0.4726562500000000000, 0.4746093750000000000, 0.4765625000000000000, 0.4785156250000000000, 0.4804687500000000000, 0.4824218750000000000, 0.4843750000000000000, 0.4863281250000000000, 0.4882812500000000000, 0.4902343750000000000, 0.4921875000000000000, 0.4941406250000000000, 0.4960937500000000000, 0.4980468750000000000, 0.5000000000000000000, 0.5019531250000000000, 0.5039062500000000000, 0.5058593750000000000, 0.5078125000000000000, 0.5097656250000000000, 0.5117187500000000000, 0.5136718750000000000, 0.5156250000000000000, 0.5175781250000000000, 0.5195312500000000000, 0.5214843750000000000, 0.5234375000000000000, 0.5253906250000000000, 0.5273437500000000000, 0.5292968750000000000, 0.5312500000000000000, 0.5332031250000000000, 0.5351562500000000000, 0.5371093750000000000, 0.5390625000000000000, 0.5410156250000000000, 0.5429687500000000000, 0.5449218750000000000, 0.5468750000000000000, 0.5488281250000000000, 0.5507812500000000000, 0.5527343750000000000, 0.5546875000000000000, 0.5566406250000000000, 0.5585937500000000000, 0.5605468750000000000, 0.5625000000000000000, 0.5644531250000000000, 0.5664062500000000000, 0.5683593750000000000, 0.5703125000000000000, 0.5722656250000000000, 0.5742187500000000000, 0.5761718750000000000, 0.5781250000000000000, 0.5800781250000000000, 0.5820312500000000000, 0.5839843750000000000, 0.5859375000000000000, 0.5878906250000000000, 0.5898437500000000000, 0.5917968750000000000, 0.5937500000000000000, 0.5957031250000000000, 0.5976562500000000000, 0.5996093750000000000, 0.6015625000000000000, 0.6035156250000000000, 0.6054687500000000000, 0.6074218750000000000, 0.6093750000000000000, 0.6113281250000000000, 0.6132812500000000000, 0.6152343750000000000, 0.6171875000000000000, 0.6191406250000000000, 0.6210937500000000000, 0.6230468750000000000, 0.6250000000000000000, 0.6269531250000000000, 0.6289062500000000000, 0.6308593750000000000, 0.6328125000000000000, 0.6347656250000000000, 0.6367187500000000000, 0.6386718750000000000, 0.6406250000000000000, 0.6425781250000000000, 0.6445312500000000000, 0.6464843750000000000, 0.6484375000000000000, 0.6503906250000000000, 0.6523437500000000000, 0.6542968750000000000, 0.6562500000000000000, 0.6582031250000000000, 0.6601562500000000000, 0.6621093750000000000, 0.6640625000000000000, 0.6660156250000000000, 0.6679687500000000000, 0.6699218750000000000, 0.6718750000000000000, 0.6738281250000000000, 0.6757812500000000000, 0.6777343750000000000, 0.6796875000000000000, 0.6816406250000000000, 0.6835937500000000000, 0.6855468750000000000, 0.6875000000000000000, 0.6894531250000000000, 0.6914062500000000000, 0.6933593750000000000, 0.6953125000000000000, 0.6972656250000000000, 0.6992187500000000000, 0.7011718750000000000, 0.7031250000000000000, 0.7050781250000000000, 0.7070312500000000000, 0.7089843750000000000, 0.7109375000000000000, 0.7128906250000000000, 0.7148437500000000000, 0.7167968750000000000, 0.7187500000000000000, 0.7207031250000000000, 0.7226562500000000000, 0.7246093750000000000, 0.7265625000000000000, 0.7285156250000000000, 0.7304687500000000000, 0.7324218750000000000, 0.7343750000000000000, 0.7363281250000000000, 0.7382812500000000000, 0.7402343750000000000, 0.7421875000000000000, 0.7441406250000000000, 0.7460937500000000000, 0.7480468750000000000, 0.7500000000000000000, 0.7519531250000000000, 0.7539062500000000000, 0.7558593750000000000, 0.7578125000000000000, 0.7597656250000000000, 0.7617187500000000000, 0.7636718750000000000, 0.7656250000000000000, 0.7675781250000000000, 0.7695312500000000000, 0.7714843750000000000, 0.7734375000000000000, 0.7753906250000000000, 0.7773437500000000000, 0.7792968750000000000, 0.7812500000000000000, 0.7832031250000000000, 0.7851562500000000000, 0.7871093750000000000, 0.7890625000000000000, 0.7910156250000000000, 0.7929687500000000000, 0.7949218750000000000, 0.7968750000000000000, 0.7988281250000000000, 0.8007812500000000000, 0.8027343750000000000, 0.8046875000000000000, 0.8066406250000000000, 0.8085937500000000000, 0.8105468750000000000, 0.8125000000000000000, 0.8144531250000000000, 0.8164062500000000000, 0.8183593750000000000, 0.8203125000000000000, 0.8222656250000000000, 0.8242187500000000000, 0.8261718750000000000, 0.8281250000000000000, 0.8300781250000000000, 0.8320312500000000000, 0.8339843750000000000, 0.8359375000000000000, 0.8378906250000000000, 0.8398437500000000000, 0.8417968750000000000, 0.8437500000000000000, 0.8457031250000000000, 0.8476562500000000000, 0.8496093750000000000, 0.8515625000000000000, 0.8535156250000000000, 0.8554687500000000000, 0.8574218750000000000, 0.8593750000000000000, 0.8613281250000000000, 0.8632812500000000000, 0.8652343750000000000, 0.8671875000000000000, 0.8691406250000000000, 0.8710937500000000000, 0.8730468750000000000, 0.8750000000000000000, 0.8769531250000000000, 0.8789062500000000000, 0.8808593750000000000, 0.8828125000000000000, 0.8847656250000000000, 0.8867187500000000000, 0.8886718750000000000, 0.8906250000000000000, 0.8925781250000000000, 0.8945312500000000000, 0.8964843750000000000, 0.8984375000000000000, 0.9003906250000000000, 0.9023437500000000000, 0.9042968750000000000, 0.9062500000000000000, 0.9082031250000000000, 0.9101562500000000000, 0.9121093750000000000, 0.9140625000000000000, 0.9160156250000000000, 0.9179687500000000000, 0.9199218750000000000, 0.9218750000000000000, 0.9238281250000000000, 0.9257812500000000000, 0.9277343750000000000, 0.9296875000000000000, 0.9316406250000000000, 0.9335937500000000000, 0.9355468750000000000, 0.9375000000000000000, 0.9394531250000000000, 0.9414062500000000000, 0.9433593750000000000, 0.9453125000000000000, 0.9472656250000000000, 0.9492187500000000000, 0.9511718750000000000, 0.9531250000000000000, 0.9550781250000000000, 0.9570312500000000000, 0.9589843750000000000, 0.9609375000000000000, 0.9628906250000000000, 0.9648437500000000000, 0.9667968750000000000, 0.9687500000000000000, 0.9707031250000000000, 0.9726562500000000000, 0.9746093750000000000, 0.9765625000000000000, 0.9785156250000000000, 0.9791718336226511443 ),
 .UNSPECIFIED. ) 
 GEOMETRIC_REPRESENTATION_ITEM ( )  RATIONAL_B_SPLINE_SURFACE ( (
 ( 1.000000000000000000, 0.9807852804032304306, 1.000000000000000000, 0.9807852804032304306, 1.000000000000000000, 0.9807852804032304306, 1.000000000000000000, 0.9807852804032304306, 1.000000000000000000, 0.9807852804032304306, 1.000000000000000000, 0.9807852804032304306, 1.000000000000000000, 0.9807852804032304306, 1.000000000000000000, 0.9807852804032304306, 1.000000000000000000, 0.9807852804032304306, 1.000000000000000000, 0.9807852804032304306, 1.000000000000000000, 0.9807852804032304306, 1.000000000000000000, 0.9807852804032304306, 1.000000000000000000, 0.9807852804032304306, 1.000000000000000000, 0.9807852804032304306, 1.000000000000000000, 0.9807852804032304306, 1.000000000000000000, 0.9807852804032304306, 1.000000000000000000, 0.9807852804032304306, 1.000000000000000000, 0.9807852804032304306, 1.000000000000000000, 0.9807852804032304306, 1.000000000000000000, 0.9807852804032304306, 1.000000000000000000, 0.9807852804032304306, 1.000000000000000000, 0.9807852804032304306, 1.000000000000000000, 0.9807852804032304306, 1.000000000000000000, 0.9807852804032304306, 1.000000000000000000, 0.9807852804032304306, 1.000000000000000000, 0.9807852804032304306, 1.000000000000000000, 0.9807852804032304306, 1.000000000000000000, 0.9807852804032304306, 1.000000000000000000, 0.9807852804032304306, 1.000000000000000000, 0.9807852804032304306, 1.000000000000000000, 0.9807852804032304306, 1.000000000000000000, 0.9807852804032304306, 1.000000000000000000, 0.9807852804032304306, 1.000000000000000000, 0.9807852804032304306, 1.000000000000000000, 0.9807852804032304306, 1.000000000000000000, 0.9807852804032304306, 1.000000000000000000, 0.9807852804032304306, 1.000000000000000000, 0.9807852804032304306, 1.000000000000000000, 0.9807852804032304306, 1.000000000000000000, 0.9807852804032304306, 1.000000000000000000, 0.9807852804032304306, 1.000000000000000000, 0.9807852804032304306, 1.000000000000000000, 0.9807852804032304306, 1.000000000000000000, 0.9807852804032304306, 1.000000000000000000, 0.9807852804032304306, 1.000000000000000000, 0.9807852804032304306, 1.000000000000000000, 0.9807852804032304306, 1.000000000000000000, 0.9807852804032304306, 1.000000000000000000, 0.9807852804032304306, 1.000000000000000000, 0.9807852804032304306, 1.000000000000000000, 0.9807852804032304306, 1.000000000000000000, 0.9807852804032304306, 1.000000000000000000, 0.9807852804032304306, 1.000000000000000000, 0.9807852804032304306, 1.000000000000000000, 0.9807852804032304306, 1.000000000000000000, 0.9807852804032304306, 1.000000000000000000, 0.9807852804032304306, 1.000000000000000000, 0.9807852804032304306, 1.000000000000000000, 0.9807852804032304306, 1.000000000000000000, 0.9807852804032304306, 1.000000000000000000, 0.9807852804032304306, 1.000000000000000000, 0.9807852804032304306, 1.000000000000000000, 0.9807852804032304306, 1.000000000000000000, 0.9807852804032304306, 1.000000000000000000, 0.9807852804032304306, 1.000000000000000000, 0.9807852804032304306, 1.000000000000000000, 0.9807852804032304306, 1.000000000000000000, 0.9807852804032304306, 1.000000000000000000, 0.9807852804032304306, 1.000000000000000000, 0.9807852804032304306, 1.000000000000000000, 0.9807852804032304306, 1.000000000000000000, 0.9807852804032304306, 1.000000000000000000, 0.9807852804032304306, 1.000000000000000000, 0.9807852804032304306, 1.000000000000000000, 0.9807852804032304306, 1.000000000000000000, 0.9807852804032304306, 1.000000000000000000, 0.9807852804032304306, 1.000000000000000000, 0.9807852804032304306, 1.000000000000000000, 0.9807852804032304306, 1.000000000000000000, 0.9807852804032304306, 1.000000000000000000, 0.9807852804032304306, 1.000000000000000000, 0.9807852804032304306, 1.000000000000000000, 0.9807852804032304306, 1.000000000000000000, 0.9807852804032304306, 1.000000000000000000, 0.9807852804032304306, 1.000000000000000000, 0.9807852804032304306, 1.000000000000000000, 0.9807852804032304306, 1.000000000000000000, 0.9807852804032304306, 1.000000000000000000, 0.9807852804032304306, 1.000000000000000000, 0.9807852804032304306, 1.000000000000000000, 0.9807852804032304306, 1.000000000000000000, 0.9807852804032304306, 1.000000000000000000, 0.9807852804032304306, 1.000000000000000000, 0.9807852804032304306, 1.000000000000000000, 0.9807852804032304306, 1.000000000000000000, 0.9807852804032304306, 1.000000000000000000, 0.9807852804032304306, 1.000000000000000000, 0.9807852804032304306, 1.000000000000000000, 0.9807852804032304306, 1.000000000000000000, 0.9807852804032304306, 1.000000000000000000, 0.9807852804032304306, 1.000000000000000000, 0.9807852804032304306, 1.000000000000000000, 0.9807852804032304306, 1.000000000000000000, 0.9807852804032304306, 1.000000000000000000, 0.9807852804032304306, 1.000000000000000000, 0.9807852804032304306, 1.000000000000000000, 0.9807852804032304306, 1.000000000000000000, 0.9807852804032304306, 1.000000000000000000, 0.9807852804032304306, 1.000000000000000000, 0.9807852804032304306, 1.000000000000000000, 0.9807852804032304306, 1.000000000000000000, 0.9807852804032304306, 1.000000000000000000, 0.9807852804032304306, 1.000000000000000000, 0.9807852804032304306, 1.000000000000000000, 0.9807852804032304306, 1.000000000000000000, 0.9807852804032304306, 1.000000000000000000, 0.9807852804032304306, 1.000000000000000000, 0.9807852804032304306, 1.000000000000000000, 0.9807852804032304306, 1.000000000000000000, 0.9807852804032304306, 1.000000000000000000, 0.9807852804032304306, 1.000000000000000000, 0.9807852804032304306, 1.000000000000000000, 0.9807852804032304306, 1.000000000000000000, 0.9807852804032304306, 1.000000000000000000, 0.9807852804032304306, 1.000000000000000000, 0.9807852804032304306, 1.000000000000000000, 0.9807852804032304306, 1.000000000000000000, 0.9807852804032304306, 1.000000000000000000, 0.9807852804032304306, 1.000000000000000000, 0.9807852804032304306, 1.000000000000000000, 0.9807852804032304306, 1.000000000000000000, 0.9807852804032304306, 1.000000000000000000, 0.9807852804032304306, 1.000000000000000000, 0.9807852804032304306, 1.000000000000000000, 0.9807852804032304306, 1.000000000000000000, 0.9807852804032304306, 1.000000000000000000, 0.9807852804032304306, 1.000000000000000000, 0.9807852804032304306, 1.000000000000000000, 0.9807852804032304306, 1.000000000000000000, 0.9807852804032304306, 1.000000000000000000, 0.9807852804032304306, 1.000000000000000000, 0.9807852804032304306, 1.000000000000000000, 0.9807852804032304306, 1.000000000000000000, 0.9807852804032304306, 1.000000000000000000, 0.9807852804032304306, 1.000000000000000000, 0.9807852804032304306, 1.000000000000000000, 0.9807852804032304306, 1.000000000000000000, 0.9807852804032304306, 1.000000000000000000, 0.9807852804032304306, 1.000000000000000000, 0.9807852804032304306, 1.000000000000000000, 0.9807852804032304306, 1.000000000000000000, 0.9807852804032304306, 1.000000000000000000, 0.9807852804032304306, 1.000000000000000000, 0.9807852804032304306, 1.000000000000000000, 0.9807852804032304306, 1.000000000000000000, 0.9807852804032304306, 1.000000000000000000, 0.9807852804032304306, 1.000000000000000000, 0.9807852804032304306, 1.000000000000000000, 0.9807852804032304306, 1.000000000000000000, 0.9807852804032304306, 1.000000000000000000, 0.9807852804032304306, 1.000000000000000000, 0.9807852804032304306, 1.000000000000000000, 0.9807852804032304306, 1.000000000000000000, 0.9807852804032304306, 1.000000000000000000, 0.9807852804032304306, 1.000000000000000000, 0.9807852804032304306, 1.000000000000000000, 0.9807852804032304306, 1.000000000000000000, 0.9807852804032304306, 1.000000000000000000, 0.9807852804032304306, 1.000000000000000000, 0.9807852804032304306, 1.000000000000000000, 0.9807852804032304306, 1.000000000000000000, 0.9807852804032304306, 1.000000000000000000, 0.9807852804032304306, 1.000000000000000000, 0.9807852804032304306, 1.000000000000000000, 0.9807852804032304306, 1.000000000000000000, 0.9807852804032304306, 1.000000000000000000, 0.9807852804032304306, 1.000000000000000000, 0.9807852804032304306, 1.000000000000000000, 0.9807852804032304306, 1.000000000000000000, 0.9807852804032304306, 1.000000000000000000, 0.9807852804032304306, 1.000000000000000000, 0.9807852804032304306, 1.000000000000000000, 0.9807852804032304306, 1.000000000000000000, 0.9807852804032304306, 1.000000000000000000, 0.9807852804032304306, 1.000000000000000000, 0.9807852804032304306, 1.000000000000000000, 0.9807852804032304306, 1.000000000000000000, 0.9807852804032304306, 1.000000000000000000, 0.9807852804032304306, 1.000000000000000000, 0.9807852804032304306, 1.000000000000000000, 0.9807852804032304306, 1.000000000000000000, 0.9807852804032304306, 1.000000000000000000, 0.9807852804032304306, 1.000000000000000000, 0.9807852804032304306, 1.000000000000000000, 0.9807852804032304306, 1.000000000000000000, 0.9807852804032304306, 1.000000000000000000, 0.9807852804032304306, 1.000000000000000000, 0.9807852804032304306, 1.000000000000000000, 0.9807852804032304306, 1.000000000000000000, 0.9807852804032304306, 1.000000000000000000, 0.9807852804032304306, 1.000000000000000000, 0.9807852804032304306, 1.000000000000000000, 0.9807852804032304306, 1.000000000000000000, 0.9807852804032304306, 1.000000000000000000, 0.9807852804032304306, 1.000000000000000000, 0.9807852804032304306, 1.000000000000000000, 0.9807852804032304306, 1.000000000000000000, 0.9807852804032304306, 1.000000000000000000, 0.9807852804032304306, 1.000000000000000000, 0.9807852804032304306, 1.000000000000000000, 0.9807852804032304306, 1.000000000000000000, 0.9807852804032304306, 1.000000000000000000, 0.9807852804032304306, 1.000000000000000000, 0.9807852804032304306, 1.000000000000000000, 0.9807852804032304306, 1.000000000000000000, 0.9807852804032304306, 1.000000000000000000, 0.9807852804032304306, 1.000000000000000000, 0.9807852804032304306, 1.000000000000000000, 0.9807852804032304306, 1.000000000000000000, 0.9807852804032304306, 1.000000000000000000, 0.9807852804032304306, 1.000000000000000000, 0.9807852804032304306, 1.000000000000000000, 0.9807852804032304306, 1.000000000000000000, 0.9807852804032304306, 1.000000000000000000, 0.9807852804032304306, 1.000000000000000000, 0.9807852804032304306, 1.000000000000000000, 0.9807852804032304306, 1.000000000000000000, 0.9807852804032304306, 1.000000000000000000, 0.9807852804032304306, 1.000000000000000000, 0.9807852804032304306, 1.000000000000000000, 0.9807852804032304306, 1.000000000000000000, 0.9807852804032304306, 1.000000000000000000, 0.9807852804032304306, 1.000000000000000000, 0.9807852804032304306, 1.000000000000000000, 0.9807852804032304306, 1.000000000000000000, 0.9807852804032304306, 1.000000000000000000, 0.9807852804032304306, 1.000000000000000000, 0.9807852804032304306, 1.000000000000000000, 0.9807852804032304306, 1.000000000000000000, 0.9807852804032304306, 1.000000000000000000, 0.9807852804032304306, 1.000000000000000000, 0.9807852804032304306, 1.000000000000000000, 0.9807852804032304306, 1.000000000000000000, 0.9807852804032304306, 1.000000000000000000, 0.9807852804032304306, 1.000000000000000000, 0.9807852804032304306, 1.000000000000000000, 0.9807852804032304306, 1.000000000000000000, 0.9807852804032304306, 1.000000000000000000, 0.9807852804032304306, 1.000000000000000000, 0.9807852804032304306, 1.000000000000000000, 0.9807852804032304306, 1.000000000000000000, 0.9807852804032304306, 1.000000000000000000, 0.9807852804032304306, 1.000000000000000000, 0.9807852804032304306, 1.000000000000000000, 0.9807852804032304306, 1.000000000000000000, 0.9807852804032304306, 1.000000000000000000, 0.9807852804032304306, 1.000000000000000000, 0.9807852804032304306, 1.000000000000000000, 0.9807852804032304306, 1.000000000000000000, 0.9807852804032304306, 1.000000000000000000, 0.9807852804032304306, 1.000000000000000000, 0.9807852804032304306, 1.000000000000000000, 0.9807852804032304306, 1.000000000000000000, 0.9807852804032304306, 1.000000000000000000, 0.9807852804032304306, 1.000000000000000000, 0.9807852804032304306, 1.000000000000000000, 0.9807852804032304306, 1.000000000000000000, 0.9807852804032304306, 1.000000000000000000, 0.9807852804032304306, 1.000000000000000000, 0.9807852804032304306, 1.000000000000000000, 0.9807852804032304306, 1.000000000000000000, 0.9807852804032304306, 1.000000000000000000, 0.9807852804032304306, 1.000000000000000000, 0.9807852804032304306, 1.000000000000000000, 0.9807852804032304306, 1.000000000000000000, 0.9807852804032304306, 1.000000000000000000, 0.9807852804032304306, 1.000000000000000000, 0.9807852804032304306, 1.000000000000000000, 0.9807852804032304306, 1.000000000000000000, 0.9807852804032304306, 1.000000000000000000, 0.9807852804032304306, 1.000000000000000000, 0.9807852804032304306, 1.000000000000000000, 0.9807852804032304306, 1.000000000000000000, 0.9807852804032304306, 1.000000000000000000, 0.9807852804032304306, 1.000000000000000000, 0.9807852804032304306, 1.000000000000000000, 0.9807852804032304306, 1.000000000000000000, 0.9807852804032304306, 1.000000000000000000, 0.9807852804032304306, 1.000000000000000000, 0.9807852804032304306, 1.000000000000000000, 0.9807852804032304306, 1.000000000000000000, 0.9807852804032304306, 1.000000000000000000, 0.9807852804032304306, 1.000000000000000000, 0.9807852804032304306, 1.000000000000000000, 0.9807852804032304306, 1.000000000000000000, 0.9807852804032304306, 1.000000000000000000, 0.9807852804032304306, 1.000000000000000000, 0.9807852804032304306, 1.000000000000000000, 0.9807852804032304306, 1.000000000000000000, 0.9807852804032304306, 1.000000000000000000, 0.9807852804032304306, 1.000000000000000000, 0.9807852804032304306, 1.000000000000000000, 0.9807852804032304306, 1.000000000000000000, 0.9807852804032304306, 1.000000000000000000, 0.9807852804032304306, 1.000000000000000000, 0.9807852804032304306, 1.000000000000000000, 0.9807852804032304306, 1.000000000000000000, 0.9807852804032304306, 1.000000000000000000, 0.9807852804032304306, 1.000000000000000000, 0.9807852804032304306, 1.000000000000000000, 0.9807852804032304306, 1.000000000000000000, 0.9807852804032304306, 1.000000000000000000, 0.9807852804032304306, 1.000000000000000000, 0.9807852804032304306, 1.000000000000000000, 0.9807852804032304306, 1.000000000000000000, 0.9807852804032304306, 1.000000000000000000, 0.9807852804032304306, 1.000000000000000000, 0.9807852804032304306, 1.000000000000000000, 0.9807852804032304306, 1.000000000000000000, 0.9807852804032304306, 1.000000000000000000, 0.9807852804032304306, 1.000000000000000000, 0.9807852804032304306, 1.000000000000000000, 0.9807852804032304306, 1.000000000000000000, 0.9807852804032304306, 1.000000000000000000, 0.9807852804032304306, 1.000000000000000000, 0.9807852804032304306, 1.000000000000000000, 0.9807852804032304306, 1.000000000000000000, 0.9807852804032304306, 1.000000000000000000, 0.9807852804032304306, 1.000000000000000000, 0.9807852804032304306, 1.000000000000000000, 0.9807852804032304306, 1.000000000000000000, 0.9807852804032304306, 1.000000000000000000, 0.9807852804032304306, 1.000000000000000000, 0.9807852804032304306, 1.000000000000000000, 0.9807852804032304306, 1.000000000000000000, 0.9807852804032304306, 1.000000000000000000, 0.9807852804032304306, 1.000000000000000000, 0.9807852804032304306, 1.000000000000000000, 0.9807852804032304306, 1.000000000000000000, 0.9807852804032304306, 1.000000000000000000, 0.9807852804032304306, 1.000000000000000000, 0.9807852804032304306, 1.000000000000000000, 0.9807852804032304306, 1.000000000000000000, 0.9807852804032304306, 1.000000000000000000, 0.9807852804032304306, 1.000000000000000000, 0.9807852804032304306, 1.000000000000000000, 0.9807852804032304306, 1.000000000000000000, 0.9807852804032304306, 1.000000000000000000, 0.9807852804032304306, 1.000000000000000000, 0.9807852804032304306, 1.000000000000000000, 0.9807852804032304306, 1.000000000000000000, 0.9807852804032304306, 1.000000000000000000, 0.9807852804032304306, 1.000000000000000000, 0.9807852804032304306, 1.000000000000000000, 0.9807852804032304306, 1.000000000000000000, 0.9807852804032304306, 1.000000000000000000, 0.9807852804032304306, 1.000000000000000000, 0.9807852804032304306, 1.000000000000000000, 0.9807852804032304306, 1.000000000000000000, 0.9807852804032304306, 1.000000000000000000, 0.9807852804032304306, 1.000000000000000000, 0.9807852804032304306, 1.000000000000000000, 0.9807852804032304306, 1.000000000000000000, 0.9807852804032304306, 1.000000000000000000, 0.9807852804032304306, 1.000000000000000000, 0.9807852804032304306, 1.000000000000000000, 0.9807852804032304306, 1.000000000000000000, 0.9807852804032304306, 1.000000000000000000, 0.9807852804032304306, 1.000000000000000000, 0.9807852804032304306, 1.000000000000000000, 0.9807852804032304306, 1.000000000000000000, 0.9807852804032304306, 1.000000000000000000, 0.9807852804032304306, 1.000000000000000000, 0.9807852804032304306, 1.000000000000000000, 0.9807852804032304306, 1.000000000000000000, 0.9807852804032304306, 1.000000000000000000, 0.9807852804032304306, 1.000000000000000000, 0.9807852804032304306, 1.000000000000000000, 0.9807852804032304306, 1.000000000000000000, 0.9807852804032304306, 1.000000000000000000, 0.9807852804032304306, 1.000000000000000000, 0.9807852804032304306, 1.000000000000000000, 0.9807852804032304306, 1.000000000000000000, 0.9807852804032304306, 1.000000000000000000, 0.9807852804032304306, 1.000000000000000000, 0.9807852804032304306, 1.000000000000000000, 0.9807852804032304306, 1.000000000000000000, 0.9807852804032304306, 1.000000000000000000, 0.9807852804032304306, 1.000000000000000000, 0.9807852804032304306, 1.000000000000000000, 0.9807852804032304306, 1.000000000000000000, 0.9807852804032304306, 1.000000000000000000, 0.9807852804032304306, 1.000000000000000000, 0.9807852804032304306, 1.000000000000000000, 0.9807852804032304306, 1.000000000000000000, 0.9807852804032304306, 1.000000000000000000, 0.9807852804032304306, 1.000000000000000000, 0.9807852804032304306, 1.000000000000000000, 0.9807852804032304306, 1.000000000000000000, 0.9807852804032304306, 1.000000000000000000, 0.9807852804032304306, 1.000000000000000000, 0.9807852804032304306, 1.000000000000000000, 0.9807852804032304306, 1.000000000000000000, 0.9807852804032304306, 1.000000000000000000, 0.9807852804032304306, 1.000000000000000000, 0.9807852804032304306, 1.000000000000000000, 0.9807852804032304306, 1.000000000000000000, 0.9807852804032304306, 1.000000000000000000, 0.9807852804032304306, 1.000000000000000000, 0.9807852804032304306, 1.000000000000000000, 0.9807852804032304306, 1.000000000000000000, 0.9807852804032304306, 1.000000000000000000, 0.9807852804032304306, 1.000000000000000000, 0.9807852804032304306, 1.000000000000000000, 0.9807852804032304306, 1.000000000000000000, 0.9807852804032304306, 1.000000000000000000, 0.9807852804032304306, 1.000000000000000000, 0.9807852804032304306, 1.000000000000000000, 0.9807852804032304306, 1.000000000000000000, 0.9807852804032304306, 1.000000000000000000, 0.9807852804032304306, 1.000000000000000000, 0.9807852804032304306, 1.000000000000000000, 0.9807852804032304306, 1.000000000000000000, 0.9807852804032304306, 1.000000000000000000, 0.9807852804032304306, 1.000000000000000000, 0.9807852804032304306, 1.000000000000000000, 0.9807852804032304306, 1.000000000000000000, 0.9807852804032304306, 1.000000000000000000, 0.9807852804032304306, 1.000000000000000000, 0.9807852804032304306, 1.000000000000000000, 0.9807852804032304306, 1.000000000000000000, 0.9807852804032304306, 1.000000000000000000, 0.9807852804032304306, 1.000000000000000000, 0.9807852804032304306, 1.000000000000000000, 0.9807852804032304306, 1.000000000000000000, 0.9807852804032304306, 1.000000000000000000, 0.9807852804032304306, 1.000000000000000000, 0.9807852804032304306, 1.000000000000000000, 0.9807852804032304306, 1.000000000000000000, 0.9807852804032304306, 1.000000000000000000, 0.9807852804032304306, 1.000000000000000000, 0.9807852804032304306, 1.000000000000000000, 0.9807852804032304306, 1.000000000000000000, 0.9807852804032304306, 1.000000000000000000, 0.9807852804032304306, 1.000000000000000000, 0.9807852804032304306, 1.000000000000000000, 0.9807852804032304306, 1.000000000000000000, 0.9807852804032304306, 1.000000000000000000, 0.9807852804032304306, 1.000000000000000000, 0.9807852804032304306, 1.000000000000000000, 0.9807852804032304306, 1.000000000000000000, 0.9807852804032304306, 1.000000000000000000, 0.9807852804032304306, 1.000000000000000000, 0.9807852804032304306, 1.000000000000000000, 0.9807852804032304306, 1.000000000000000000, 0.9807852804032304306, 1.000000000000000000, 0.9807852804032304306, 1.000000000000000000, 0.9807852804032304306, 1.000000000000000000, 0.9807852804032304306, 1.000000000000000000, 0.9807852804032304306, 1.000000000000000000, 0.9807852804032304306, 1.000000000000000000, 0.9807852804032304306, 1.000000000000000000, 0.9807852804032304306, 1.000000000000000000, 0.9807852804032304306, 1.000000000000000000, 0.9807852804032304306, 1.000000000000000000, 0.9807852804032304306, 1.000000000000000000, 0.9807852804032304306, 1.000000000000000000, 0.9807852804032304306, 1.000000000000000000, 0.9807852804032304306, 1.000000000000000000, 0.9807852804032304306, 1.000000000000000000, 0.9807852804032304306, 1.000000000000000000, 0.9807852804032304306, 1.000000000000000000, 0.9807852804032304306, 1.000000000000000000, 0.9807852804032304306, 1.000000000000000000, 0.9807852804032304306, 1.000000000000000000, 0.9807852804032304306, 1.000000000000000000, 0.9807852804032304306, 1.000000000000000000, 0.9807852804032304306, 1.000000000000000000, 0.9807852804032304306, 1.000000000000000000, 0.9807852804032304306, 1.000000000000000000, 0.9807852804032304306, 1.000000000000000000, 0.9807852804032304306, 1.000000000000000000, 0.9807852804032304306, 1.000000000000000000, 0.9807852804032304306, 1.000000000000000000, 0.9807852804032304306, 1.000000000000000000, 0.9807852804032304306, 1.000000000000000000, 0.9807852804032304306, 1.000000000000000000, 0.9807852804032304306, 1.000000000000000000, 0.9807852804032304306, 1.000000000000000000, 0.9807852804032304306, 1.000000000000000000, 0.9807852804032304306, 1.000000000000000000, 0.9807852804032304306, 1.000000000000000000, 0.9807852804032304306, 1.000000000000000000, 0.9807852804032304306, 1.000000000000000000, 0.9807852804032304306, 1.000000000000000000, 0.9807852804032304306, 1.000000000000000000, 0.9807852804032304306, 1.000000000000000000, 0.9807852804032304306, 1.000000000000000000, 0.9807852804032304306, 1.000000000000000000, 0.9807852804032304306, 1.000000000000000000, 0.9807852804032304306, 1.000000000000000000, 0.9935442612832132703, 0.9914265054518418552),
 ( 1.000000000000000000, 0.9807852804032304306, 1.000000000000000000, 0.9807852804032304306, 1.000000000000000000, 0.9807852804032304306, 1.000000000000000000, 0.9807852804032304306, 1.000000000000000000, 0.9807852804032304306, 1.000000000000000000, 0.9807852804032304306, 1.000000000000000000, 0.9807852804032304306, 1.000000000000000000, 0.9807852804032304306, 1.000000000000000000, 0.9807852804032304306, 1.000000000000000000, 0.9807852804032304306, 1.000000000000000000, 0.9807852804032304306, 1.000000000000000000, 0.9807852804032304306, 1.000000000000000000, 0.9807852804032304306, 1.000000000000000000, 0.9807852804032304306, 1.000000000000000000, 0.9807852804032304306, 1.000000000000000000, 0.9807852804032304306, 1.000000000000000000, 0.9807852804032304306, 1.000000000000000000, 0.9807852804032304306, 1.000000000000000000, 0.9807852804032304306, 1.000000000000000000, 0.9807852804032304306, 1.000000000000000000, 0.9807852804032304306, 1.000000000000000000, 0.9807852804032304306, 1.000000000000000000, 0.9807852804032304306, 1.000000000000000000, 0.9807852804032304306, 1.000000000000000000, 0.9807852804032304306, 1.000000000000000000, 0.9807852804032304306, 1.000000000000000000, 0.9807852804032304306, 1.000000000000000000, 0.9807852804032304306, 1.000000000000000000, 0.9807852804032304306, 1.000000000000000000, 0.9807852804032304306, 1.000000000000000000, 0.9807852804032304306, 1.000000000000000000, 0.9807852804032304306, 1.000000000000000000, 0.9807852804032304306, 1.000000000000000000, 0.9807852804032304306, 1.000000000000000000, 0.9807852804032304306, 1.000000000000000000, 0.9807852804032304306, 1.000000000000000000, 0.9807852804032304306, 1.000000000000000000, 0.9807852804032304306, 1.000000000000000000, 0.9807852804032304306, 1.000000000000000000, 0.9807852804032304306, 1.000000000000000000, 0.9807852804032304306, 1.000000000000000000, 0.9807852804032304306, 1.000000000000000000, 0.9807852804032304306, 1.000000000000000000, 0.9807852804032304306, 1.000000000000000000, 0.9807852804032304306, 1.000000000000000000, 0.9807852804032304306, 1.000000000000000000, 0.9807852804032304306, 1.000000000000000000, 0.9807852804032304306, 1.000000000000000000, 0.9807852804032304306, 1.000000000000000000, 0.9807852804032304306, 1.000000000000000000, 0.9807852804032304306, 1.000000000000000000, 0.9807852804032304306, 1.000000000000000000, 0.9807852804032304306, 1.000000000000000000, 0.9807852804032304306, 1.000000000000000000, 0.9807852804032304306, 1.000000000000000000, 0.9807852804032304306, 1.000000000000000000, 0.9807852804032304306, 1.000000000000000000, 0.9807852804032304306, 1.000000000000000000, 0.9807852804032304306, 1.000000000000000000, 0.9807852804032304306, 1.000000000000000000, 0.9807852804032304306, 1.000000000000000000, 0.9807852804032304306, 1.000000000000000000, 0.9807852804032304306, 1.000000000000000000, 0.9807852804032304306, 1.000000000000000000, 0.9807852804032304306, 1.000000000000000000, 0.9807852804032304306, 1.000000000000000000, 0.9807852804032304306, 1.000000000000000000, 0.9807852804032304306, 1.000000000000000000, 0.9807852804032304306, 1.000000000000000000, 0.9807852804032304306, 1.000000000000000000, 0.9807852804032304306, 1.000000000000000000, 0.9807852804032304306, 1.000000000000000000, 0.9807852804032304306, 1.000000000000000000, 0.9807852804032304306, 1.000000000000000000, 0.9807852804032304306, 1.000000000000000000, 0.9807852804032304306, 1.000000000000000000, 0.9807852804032304306, 1.000000000000000000, 0.9807852804032304306, 1.000000000000000000, 0.9807852804032304306, 1.000000000000000000, 0.9807852804032304306, 1.000000000000000000, 0.9807852804032304306, 1.000000000000000000, 0.9807852804032304306, 1.000000000000000000, 0.9807852804032304306, 1.000000000000000000, 0.9807852804032304306, 1.000000000000000000, 0.9807852804032304306, 1.000000000000000000, 0.9807852804032304306, 1.000000000000000000, 0.9807852804032304306, 1.000000000000000000, 0.9807852804032304306, 1.000000000000000000, 0.9807852804032304306, 1.000000000000000000, 0.9807852804032304306, 1.000000000000000000, 0.9807852804032304306, 1.000000000000000000, 0.9807852804032304306, 1.000000000000000000, 0.9807852804032304306, 1.000000000000000000, 0.9807852804032304306, 1.000000000000000000, 0.9807852804032304306, 1.000000000000000000, 0.9807852804032304306, 1.000000000000000000, 0.9807852804032304306, 1.000000000000000000, 0.9807852804032304306, 1.000000000000000000, 0.9807852804032304306, 1.000000000000000000, 0.9807852804032304306, 1.000000000000000000, 0.9807852804032304306, 1.000000000000000000, 0.9807852804032304306, 1.000000000000000000, 0.9807852804032304306, 1.000000000000000000, 0.9807852804032304306, 1.000000000000000000, 0.9807852804032304306, 1.000000000000000000, 0.9807852804032304306, 1.000000000000000000, 0.9807852804032304306, 1.000000000000000000, 0.9807852804032304306, 1.000000000000000000, 0.9807852804032304306, 1.000000000000000000, 0.9807852804032304306, 1.000000000000000000, 0.9807852804032304306, 1.000000000000000000, 0.9807852804032304306, 1.000000000000000000, 0.9807852804032304306, 1.000000000000000000, 0.9807852804032304306, 1.000000000000000000, 0.9807852804032304306, 1.000000000000000000, 0.9807852804032304306, 1.000000000000000000, 0.9807852804032304306, 1.000000000000000000, 0.9807852804032304306, 1.000000000000000000, 0.9807852804032304306, 1.000000000000000000, 0.9807852804032304306, 1.000000000000000000, 0.9807852804032304306, 1.000000000000000000, 0.9807852804032304306, 1.000000000000000000, 0.9807852804032304306, 1.000000000000000000, 0.9807852804032304306, 1.000000000000000000, 0.9807852804032304306, 1.000000000000000000, 0.9807852804032304306, 1.000000000000000000, 0.9807852804032304306, 1.000000000000000000, 0.9807852804032304306, 1.000000000000000000, 0.9807852804032304306, 1.000000000000000000, 0.9807852804032304306, 1.000000000000000000, 0.9807852804032304306, 1.000000000000000000, 0.9807852804032304306, 1.000000000000000000, 0.9807852804032304306, 1.000000000000000000, 0.9807852804032304306, 1.000000000000000000, 0.9807852804032304306, 1.000000000000000000, 0.9807852804032304306, 1.000000000000000000, 0.9807852804032304306, 1.000000000000000000, 0.9807852804032304306, 1.000000000000000000, 0.9807852804032304306, 1.000000000000000000, 0.9807852804032304306, 1.000000000000000000, 0.9807852804032304306, 1.000000000000000000, 0.9807852804032304306, 1.000000000000000000, 0.9807852804032304306, 1.000000000000000000, 0.9807852804032304306, 1.000000000000000000, 0.9807852804032304306, 1.000000000000000000, 0.9807852804032304306, 1.000000000000000000, 0.9807852804032304306, 1.000000000000000000, 0.9807852804032304306, 1.000000000000000000, 0.9807852804032304306, 1.000000000000000000, 0.9807852804032304306, 1.000000000000000000, 0.9807852804032304306, 1.000000000000000000, 0.9807852804032304306, 1.000000000000000000, 0.9807852804032304306, 1.000000000000000000, 0.9807852804032304306, 1.000000000000000000, 0.9807852804032304306, 1.000000000000000000, 0.9807852804032304306, 1.000000000000000000, 0.9807852804032304306, 1.000000000000000000, 0.9807852804032304306, 1.000000000000000000, 0.9807852804032304306, 1.000000000000000000, 0.9807852804032304306, 1.000000000000000000, 0.9807852804032304306, 1.000000000000000000, 0.9807852804032304306, 1.000000000000000000, 0.9807852804032304306, 1.000000000000000000, 0.9807852804032304306, 1.000000000000000000, 0.9807852804032304306, 1.000000000000000000, 0.9807852804032304306, 1.000000000000000000, 0.9807852804032304306, 1.000000000000000000, 0.9807852804032304306, 1.000000000000000000, 0.9807852804032304306, 1.000000000000000000, 0.9807852804032304306, 1.000000000000000000, 0.9807852804032304306, 1.000000000000000000, 0.9807852804032304306, 1.000000000000000000, 0.9807852804032304306, 1.000000000000000000, 0.9807852804032304306, 1.000000000000000000, 0.9807852804032304306, 1.000000000000000000, 0.9807852804032304306, 1.000000000000000000, 0.9807852804032304306, 1.000000000000000000, 0.9807852804032304306, 1.000000000000000000, 0.9807852804032304306, 1.000000000000000000, 0.9807852804032304306, 1.000000000000000000, 0.9807852804032304306, 1.000000000000000000, 0.9807852804032304306, 1.000000000000000000, 0.9807852804032304306, 1.000000000000000000, 0.9807852804032304306, 1.000000000000000000, 0.9807852804032304306, 1.000000000000000000, 0.9807852804032304306, 1.000000000000000000, 0.9807852804032304306, 1.000000000000000000, 0.9807852804032304306, 1.000000000000000000, 0.9807852804032304306, 1.000000000000000000, 0.9807852804032304306, 1.000000000000000000, 0.9807852804032304306, 1.000000000000000000, 0.9807852804032304306, 1.000000000000000000, 0.9807852804032304306, 1.000000000000000000, 0.9807852804032304306, 1.000000000000000000, 0.9807852804032304306, 1.000000000000000000, 0.9807852804032304306, 1.000000000000000000, 0.9807852804032304306, 1.000000000000000000, 0.9807852804032304306, 1.000000000000000000, 0.9807852804032304306, 1.000000000000000000, 0.9807852804032304306, 1.000000000000000000, 0.9807852804032304306, 1.000000000000000000, 0.9807852804032304306, 1.000000000000000000, 0.9807852804032304306, 1.000000000000000000, 0.9807852804032304306, 1.000000000000000000, 0.9807852804032304306, 1.000000000000000000, 0.9807852804032304306, 1.000000000000000000, 0.9807852804032304306, 1.000000000000000000, 0.9807852804032304306, 1.000000000000000000, 0.9807852804032304306, 1.000000000000000000, 0.9807852804032304306, 1.000000000000000000, 0.9807852804032304306, 1.000000000000000000, 0.9807852804032304306, 1.000000000000000000, 0.9807852804032304306, 1.000000000000000000, 0.9807852804032304306, 1.000000000000000000, 0.9807852804032304306, 1.000000000000000000, 0.9807852804032304306, 1.000000000000000000, 0.9807852804032304306, 1.000000000000000000, 0.9807852804032304306, 1.000000000000000000, 0.9807852804032304306, 1.000000000000000000, 0.9807852804032304306, 1.000000000000000000, 0.9807852804032304306, 1.000000000000000000, 0.9807852804032304306, 1.000000000000000000, 0.9807852804032304306, 1.000000000000000000, 0.9807852804032304306, 1.000000000000000000, 0.9807852804032304306, 1.000000000000000000, 0.9807852804032304306, 1.000000000000000000, 0.9807852804032304306, 1.000000000000000000, 0.9807852804032304306, 1.000000000000000000, 0.9807852804032304306, 1.000000000000000000, 0.9807852804032304306, 1.000000000000000000, 0.9807852804032304306, 1.000000000000000000, 0.9807852804032304306, 1.000000000000000000, 0.9807852804032304306, 1.000000000000000000, 0.9807852804032304306, 1.000000000000000000, 0.9807852804032304306, 1.000000000000000000, 0.9807852804032304306, 1.000000000000000000, 0.9807852804032304306, 1.000000000000000000, 0.9807852804032304306, 1.000000000000000000, 0.9807852804032304306, 1.000000000000000000, 0.9807852804032304306, 1.000000000000000000, 0.9807852804032304306, 1.000000000000000000, 0.9807852804032304306, 1.000000000000000000, 0.9807852804032304306, 1.000000000000000000, 0.9807852804032304306, 1.000000000000000000, 0.9807852804032304306, 1.000000000000000000, 0.9807852804032304306, 1.000000000000000000, 0.9807852804032304306, 1.000000000000000000, 0.9807852804032304306, 1.000000000000000000, 0.9807852804032304306, 1.000000000000000000, 0.9807852804032304306, 1.000000000000000000, 0.9807852804032304306, 1.000000000000000000, 0.9807852804032304306, 1.000000000000000000, 0.9807852804032304306, 1.000000000000000000, 0.9807852804032304306, 1.000000000000000000, 0.9807852804032304306, 1.000000000000000000, 0.9807852804032304306, 1.000000000000000000, 0.9807852804032304306, 1.000000000000000000, 0.9807852804032304306, 1.000000000000000000, 0.9807852804032304306, 1.000000000000000000, 0.9807852804032304306, 1.000000000000000000, 0.9807852804032304306, 1.000000000000000000, 0.9807852804032304306, 1.000000000000000000, 0.9807852804032304306, 1.000000000000000000, 0.9807852804032304306, 1.000000000000000000, 0.9807852804032304306, 1.000000000000000000, 0.9807852804032304306, 1.000000000000000000, 0.9807852804032304306, 1.000000000000000000, 0.9807852804032304306, 1.000000000000000000, 0.9807852804032304306, 1.000000000000000000, 0.9807852804032304306, 1.000000000000000000, 0.9807852804032304306, 1.000000000000000000, 0.9807852804032304306, 1.000000000000000000, 0.9807852804032304306, 1.000000000000000000, 0.9807852804032304306, 1.000000000000000000, 0.9807852804032304306, 1.000000000000000000, 0.9807852804032304306, 1.000000000000000000, 0.9807852804032304306, 1.000000000000000000, 0.9807852804032304306, 1.000000000000000000, 0.9807852804032304306, 1.000000000000000000, 0.9807852804032304306, 1.000000000000000000, 0.9807852804032304306, 1.000000000000000000, 0.9807852804032304306, 1.000000000000000000, 0.9807852804032304306, 1.000000000000000000, 0.9807852804032304306, 1.000000000000000000, 0.9807852804032304306, 1.000000000000000000, 0.9807852804032304306, 1.000000000000000000, 0.9807852804032304306, 1.000000000000000000, 0.9807852804032304306, 1.000000000000000000, 0.9807852804032304306, 1.000000000000000000, 0.9807852804032304306, 1.000000000000000000, 0.9807852804032304306, 1.000000000000000000, 0.9807852804032304306, 1.000000000000000000, 0.9807852804032304306, 1.000000000000000000, 0.9807852804032304306, 1.000000000000000000, 0.9807852804032304306, 1.000000000000000000, 0.9807852804032304306, 1.000000000000000000, 0.9807852804032304306, 1.000000000000000000, 0.9807852804032304306, 1.000000000000000000, 0.9807852804032304306, 1.000000000000000000, 0.9807852804032304306, 1.000000000000000000, 0.9807852804032304306, 1.000000000000000000, 0.9807852804032304306, 1.000000000000000000, 0.9807852804032304306, 1.000000000000000000, 0.9807852804032304306, 1.000000000000000000, 0.9807852804032304306, 1.000000000000000000, 0.9807852804032304306, 1.000000000000000000, 0.9807852804032304306, 1.000000000000000000, 0.9807852804032304306, 1.000000000000000000, 0.9807852804032304306, 1.000000000000000000, 0.9807852804032304306, 1.000000000000000000, 0.9807852804032304306, 1.000000000000000000, 0.9807852804032304306, 1.000000000000000000, 0.9807852804032304306, 1.000000000000000000, 0.9807852804032304306, 1.000000000000000000, 0.9807852804032304306, 1.000000000000000000, 0.9807852804032304306, 1.000000000000000000, 0.9807852804032304306, 1.000000000000000000, 0.9807852804032304306, 1.000000000000000000, 0.9807852804032304306, 1.000000000000000000, 0.9807852804032304306, 1.000000000000000000, 0.9807852804032304306, 1.000000000000000000, 0.9807852804032304306, 1.000000000000000000, 0.9807852804032304306, 1.000000000000000000, 0.9807852804032304306, 1.000000000000000000, 0.9807852804032304306, 1.000000000000000000, 0.9807852804032304306, 1.000000000000000000, 0.9807852804032304306, 1.000000000000000000, 0.9807852804032304306, 1.000000000000000000, 0.9807852804032304306, 1.000000000000000000, 0.9807852804032304306, 1.000000000000000000, 0.9807852804032304306, 1.000000000000000000, 0.9807852804032304306, 1.000000000000000000, 0.9807852804032304306, 1.000000000000000000, 0.9807852804032304306, 1.000000000000000000, 0.9807852804032304306, 1.000000000000000000, 0.9807852804032304306, 1.000000000000000000, 0.9807852804032304306, 1.000000000000000000, 0.9807852804032304306, 1.000000000000000000, 0.9807852804032304306, 1.000000000000000000, 0.9807852804032304306, 1.000000000000000000, 0.9807852804032304306, 1.000000000000000000, 0.9807852804032304306, 1.000000000000000000, 0.9807852804032304306, 1.000000000000000000, 0.9807852804032304306, 1.000000000000000000, 0.9807852804032304306, 1.000000000000000000, 0.9807852804032304306, 1.000000000000000000, 0.9807852804032304306, 1.000000000000000000, 0.9807852804032304306, 1.000000000000000000, 0.9807852804032304306, 1.000000000000000000, 0.9807852804032304306, 1.000000000000000000, 0.9807852804032304306, 1.000000000000000000, 0.9807852804032304306, 1.000000000000000000, 0.9807852804032304306, 1.000000000000000000, 0.9807852804032304306, 1.000000000000000000, 0.9807852804032304306, 1.000000000000000000, 0.9807852804032304306, 1.000000000000000000, 0.9807852804032304306, 1.000000000000000000, 0.9807852804032304306, 1.000000000000000000, 0.9807852804032304306, 1.000000000000000000, 0.9807852804032304306, 1.000000000000000000, 0.9807852804032304306, 1.000000000000000000, 0.9807852804032304306, 1.000000000000000000, 0.9807852804032304306, 1.000000000000000000, 0.9807852804032304306, 1.000000000000000000, 0.9807852804032304306, 1.000000000000000000, 0.9807852804032304306, 1.000000000000000000, 0.9807852804032304306, 1.000000000000000000, 0.9807852804032304306, 1.000000000000000000, 0.9807852804032304306, 1.000000000000000000, 0.9807852804032304306, 1.000000000000000000, 0.9807852804032304306, 1.000000000000000000, 0.9807852804032304306, 1.000000000000000000, 0.9807852804032304306, 1.000000000000000000, 0.9807852804032304306, 1.000000000000000000, 0.9807852804032304306, 1.000000000000000000, 0.9807852804032304306, 1.000000000000000000, 0.9807852804032304306, 1.000000000000000000, 0.9807852804032304306, 1.000000000000000000, 0.9807852804032304306, 1.000000000000000000, 0.9807852804032304306, 1.000000000000000000, 0.9807852804032304306, 1.000000000000000000, 0.9807852804032304306, 1.000000000000000000, 0.9807852804032304306, 1.000000000000000000, 0.9807852804032304306, 1.000000000000000000, 0.9807852804032304306, 1.000000000000000000, 0.9807852804032304306, 1.000000000000000000, 0.9807852804032304306, 1.000000000000000000, 0.9807852804032304306, 1.000000000000000000, 0.9807852804032304306, 1.000000000000000000, 0.9807852804032304306, 1.000000000000000000, 0.9807852804032304306, 1.000000000000000000, 0.9807852804032304306, 1.000000000000000000, 0.9807852804032304306, 1.000000000000000000, 0.9807852804032304306, 1.000000000000000000, 0.9807852804032304306, 1.000000000000000000, 0.9807852804032304306, 1.000000000000000000, 0.9807852804032304306, 1.000000000000000000, 0.9807852804032304306, 1.000000000000000000, 0.9807852804032304306, 1.000000000000000000, 0.9807852804032304306, 1.000000000000000000, 0.9807852804032304306, 1.000000000000000000, 0.9807852804032304306, 1.000000000000000000, 0.9807852804032304306, 1.000000000000000000, 0.9807852804032304306, 1.000000000000000000, 0.9807852804032304306, 1.000000000000000000, 0.9807852804032304306, 1.000000000000000000, 0.9807852804032304306, 1.000000000000000000, 0.9807852804032304306, 1.000000000000000000, 0.9807852804032304306, 1.000000000000000000, 0.9807852804032304306, 1.000000000000000000, 0.9807852804032304306, 1.000000000000000000, 0.9807852804032304306, 1.000000000000000000, 0.9807852804032304306, 1.000000000000000000, 0.9807852804032304306, 1.000000000000000000, 0.9807852804032304306, 1.000000000000000000, 0.9807852804032304306, 1.000000000000000000, 0.9807852804032304306, 1.000000000000000000, 0.9807852804032304306, 1.000000000000000000, 0.9807852804032304306, 1.000000000000000000, 0.9807852804032304306, 1.000000000000000000, 0.9807852804032304306, 1.000000000000000000, 0.9807852804032304306, 1.000000000000000000, 0.9807852804032304306, 1.000000000000000000, 0.9807852804032304306, 1.000000000000000000, 0.9807852804032304306, 1.000000000000000000, 0.9807852804032304306, 1.000000000000000000, 0.9807852804032304306, 1.000000000000000000, 0.9807852804032304306, 1.000000000000000000, 0.9807852804032304306, 1.000000000000000000, 0.9807852804032304306, 1.000000000000000000, 0.9807852804032304306, 1.000000000000000000, 0.9807852804032304306, 1.000000000000000000, 0.9807852804032304306, 1.000000000000000000, 0.9807852804032304306, 1.000000000000000000, 0.9807852804032304306, 1.000000000000000000, 0.9807852804032304306, 1.000000000000000000, 0.9807852804032304306, 1.000000000000000000, 0.9807852804032304306, 1.000000000000000000, 0.9807852804032304306, 1.000000000000000000, 0.9807852804032304306, 1.000000000000000000, 0.9807852804032304306, 1.000000000000000000, 0.9807852804032304306, 1.000000000000000000, 0.9807852804032304306, 1.000000000000000000, 0.9807852804032304306, 1.000000000000000000, 0.9807852804032304306, 1.000000000000000000, 0.9807852804032304306, 1.000000000000000000, 0.9807852804032304306, 1.000000000000000000, 0.9807852804032304306, 1.000000000000000000, 0.9807852804032304306, 1.000000000000000000, 0.9807852804032304306, 1.000000000000000000, 0.9807852804032304306, 1.000000000000000000, 0.9807852804032304306, 1.000000000000000000, 0.9807852804032304306, 1.000000000000000000, 0.9807852804032304306, 1.000000000000000000, 0.9807852804032304306, 1.000000000000000000, 0.9807852804032304306, 1.000000000000000000, 0.9807852804032304306, 1.000000000000000000, 0.9807852804032304306, 1.000000000000000000, 0.9807852804032304306, 1.000000000000000000, 0.9807852804032304306, 1.000000000000000000, 0.9807852804032304306, 1.000000000000000000, 0.9807852804032304306, 1.000000000000000000, 0.9807852804032304306, 1.000000000000000000, 0.9807852804032304306, 1.000000000000000000, 0.9807852804032304306, 1.000000000000000000, 0.9807852804032304306, 1.000000000000000000, 0.9807852804032304306, 1.000000000000000000, 0.9807852804032304306, 1.000000000000000000, 0.9807852804032304306, 1.000000000000000000, 0.9807852804032304306, 1.000000000000000000, 0.9807852804032304306, 1.000000000000000000, 0.9807852804032304306, 1.000000000000000000, 0.9807852804032304306, 1.000000000000000000, 0.9807852804032304306, 1.000000000000000000, 0.9807852804032304306, 1.000000000000000000, 0.9807852804032304306, 1.000000000000000000, 0.9807852804032304306, 1.000000000000000000, 0.9807852804032304306, 1.000000000000000000, 0.9807852804032304306, 1.000000000000000000, 0.9807852804032304306, 1.000000000000000000, 0.9807852804032304306, 1.000000000000000000, 0.9807852804032304306, 1.000000000000000000, 0.9807852804032304306, 1.000000000000000000, 0.9807852804032304306, 1.000000000000000000, 0.9807852804032304306, 1.000000000000000000, 0.9807852804032304306, 1.000000000000000000, 0.9807852804032304306, 1.000000000000000000, 0.9807852804032304306, 1.000000000000000000, 0.9807852804032304306, 1.000000000000000000, 0.9807852804032304306, 1.000000000000000000, 0.9807852804032304306, 1.000000000000000000, 0.9807852804032304306, 1.000000000000000000, 0.9807852804032304306, 1.000000000000000000, 0.9807852804032304306, 1.000000000000000000, 0.9807852804032304306, 1.000000000000000000, 0.9807852804032304306, 1.000000000000000000, 0.9807852804032304306, 1.000000000000000000, 0.9807852804032304306, 1.000000000000000000, 0.9807852804032304306, 1.000000000000000000, 0.9807852804032304306, 1.000000000000000000, 0.9807852804032304306, 1.000000000000000000, 0.9935442612832132703, 0.9914265054518418552) ) ) 
 REPRESENTATION_ITEM ( '' )  SURFACE ( )  );
#5023 = CARTESIAN_POINT ( 'NONE',  ( -35.09675569278793006, 233.4948905683720284, -15.47720386886985544 ) ) ;
#5024 = CARTESIAN_POINT ( 'NONE',  ( -14.48388495494899963, 367.9323905683720000, 9.489475012073732785 ) ) ;
#5025 = VERTEX_POINT ( 'NONE', #15411 ) ;
#5026 = CARTESIAN_POINT ( 'NONE',  ( -45.43829269268872650, 523.5573905683721705, -3.332260488124726194 ) ) ;
#5027 = EDGE_LOOP ( 'NONE', ( #5294, #6587, #12650, #8017, #11006, #18386 ) ) ;
#5028 = CARTESIAN_POINT ( 'NONE',  ( -38.17536295476245556, 446.9323905683720568, 14.20200298773971781 ) ) ;
#5029 = CARTESIAN_POINT ( 'NONE',  ( -42.88789093042845479, 524.8073905683720568, 9.489475012073736337 ) ) ;
#5030 = LINE ( 'NONE', #18331, #2094 ) ;
#5031 = CARTESIAN_POINT ( 'NONE',  ( -45.64106924314019409, 496.3073905601784759, -11.32908994701042538 ) ) ;
#5032 = CARTESIAN_POINT ( 'NONE',  ( -13.20868407381887444, 479.4948905683720000, -6.410867750099233042 ) ) ;
#5033 = ORIENTED_EDGE ( 'NONE', *, *, #4335, .F. ) ;
#5034 = CARTESIAN_POINT ( 'NONE',  ( -16.84014894278200458, 507.6198905683720000, 11.84573899990672530 ) ) ;
#5035 = CARTESIAN_POINT ( 'NONE',  ( -15.73313710990876402, 47.36853976159893165, -47.88030834489089926 ) ) ;
#5036 = CARTESIAN_POINT ( 'NONE',  ( -42.82802356641967378, 450.7448905765656377, -14.14213562373094746 ) ) ;
#5037 = CARTESIAN_POINT ( 'NONE',  ( -3.557538378468059575E-17, -0.6346842323199916036, 6.500000000000000000 ) ) ;
#5038 = EDGE_CURVE ( 'NONE', #1162, #5907, #10513, .T. ) ;
#5039 = CARTESIAN_POINT ( 'NONE',  ( 40.42502041961814996, 180.1716627696692967, 40.00000000000000000 ) ) ;
#5040 = CARTESIAN_POINT ( 'NONE',  ( 65.85920792673738333, 160.1716627696692683, -40.00000000000000000 ) ) ;
#5041 = FACE_OUTER_BOUND ( 'NONE', #3827, .T. ) ;
#5042 = CARTESIAN_POINT ( 'NONE',  ( -28.68588794268869435, 188.9102039777116602, 0.000000000000000000 ) ) ;
#5043 = CARTESIAN_POINT ( 'NONE',  ( -48.68588794268862330, 436.9323905601784759, -3.978247347593371508 ) ) ;
#5044 = CARTESIAN_POINT ( 'NONE',  ( -43.52287249567941529, 200.6548609068916278, -2.226397062484288814 ) ) ;
#5045 = CARTESIAN_POINT ( 'NONE',  ( -25.35362745456398414, 292.5573905683720568, -16.75240474999999307 ) ) ;
#5046 = CARTESIAN_POINT ( 'NONE',  ( -45.64106924314020119, 528.1823905601785327, 11.32908994701042538 ) ) ;
#5047 = CARTESIAN_POINT ( 'NONE',  ( -17.35679799567828852, 273.8073905601784759, -16.95518130045146421 ) ) ;
#5048 = CYLINDRICAL_SURFACE ( 'NONE', #8523, 10.00000000000000178 ) ;
#5049 = CARTESIAN_POINT ( 'NONE',  ( -45.43829269268870519, 295.3698905683720568, 0.000000000000000000 ) ) ;
#5050 = CARTESIAN_POINT ( 'NONE',  ( -44.16309181155857999, 505.9948905683720000, 6.410867750099241924 ) ) ;
#5051 = EDGE_CURVE ( 'NONE', #5934, #15977, #13892, .T. ) ;
#5052 = CIRCLE ( 'NONE', #6777, 6.500000000000000888 ) ;
#5053 = CARTESIAN_POINT ( 'NONE',  ( -10.76731745429009912, 56.85652257517428865, 118.3724535612433186 ) ) ;
#5054 = EDGE_LOOP ( 'NONE', ( #6322, #17971 ) ) ;
#5055 = CARTESIAN_POINT ( 'NONE',  ( -42.88789093042844769, 464.4323905683720000, -9.489475012073736337 ) ) ;
#5056 = FACE_OUTER_BOUND ( 'NONE', #7657, .T. ) ;
#5057 = CARTESIAN_POINT ( 'NONE',  ( -25.35362745456398059, 271.0573905683720000, -16.75240474999999307 ) ) ;
#5058 = VERTEX_POINT ( 'NONE', #17136 ) ;
#5059 = DIRECTION ( 'NONE',  ( -1.000000000000000000, -0.000000000000000000, -0.000000000000000000 ) ) ;
#5060 = VECTOR ( 'NONE', #7134, 1000.000000000000000 ) ;
#5061 = CARTESIAN_POINT ( 'NONE',  ( -40.53162694259542320, 254.1198905683720284, -11.84573899990672707 ) ) ;
#5062 = CARTESIAN_POINT ( 'NONE',  ( -11.73070664223723192, 246.0573905765656377, 11.32908994701042005 ) ) ;
#5063 = LINE ( 'NONE', #14927, #6543 ) ;
#5064 = CARTESIAN_POINT ( 'NONE',  ( -17.35679799567827430, 230.6823905601784759, 16.95518130045146421 ) ) ;
#5065 = DIRECTION ( 'NONE',  ( 0.000000000000000000, 0.000000000000000000, 1.000000000000000000 ) ) ;
#5066 = CARTESIAN_POINT ( 'NONE',  ( -19.19641293061497578, 270.4323905683720000, -14.20200298773971603 ) ) ;
#5067 = CARTESIAN_POINT ( 'NONE',  ( -14.48388495494899963, 361.3073905683721136, -9.489475012073736337 ) ) ;
#5068 = ADVANCED_FACE ( 'NONE', ( #2316 ), #2526, .T. ) ;
#5069 = VECTOR ( 'NONE', #15022, 1000.000000000000000 ) ;
#5070 = CARTESIAN_POINT ( 'NONE',  ( -48.68588794268887199, 277.5573905601784190, 3.978247347592742678 ) ) ;
#5071 = DIRECTION ( 'NONE',  ( 0.000000000000000000, 0.000000000000000000, -1.000000000000000000 ) ) ;
#5072 = VECTOR ( 'NONE', #1570, 1000.000000000000000 ) ;
#5073 = CARTESIAN_POINT ( 'NONE',  ( -11.93348319268872970, 428.8698905683720568, -2.051577885510841163E-15 ) ) ;
#5074 = DIRECTION ( 'NONE',  ( 0.000000000000000000, 0.000000000000000000, 1.000000000000000000 ) ) ;
#5075 = ORIENTED_EDGE ( 'NONE', *, *, #1422, .F. ) ;
#5076 = CARTESIAN_POINT ( 'NONE',  ( -8.685887942688729879, 431.9323905601784190, 3.978247347593161010 ) ) ;
#5077 = EDGE_CURVE ( 'NONE', #9549, #20916, #15731, .T. ) ;
#5078 = ORIENTED_EDGE ( 'NONE', *, *, #20990, .T. ) ;
#5079 = CARTESIAN_POINT ( 'NONE',  ( 6.416697501590670427, 172.9933428177121471, 45.00000000000000000 ) ) ;
#5080 = ORIENTED_EDGE ( 'NONE', *, *, #4805, .F. ) ;
#5081 = ORIENTED_EDGE ( 'NONE', *, *, #3716, .F. ) ;
#5082 = CARTESIAN_POINT ( 'NONE',  ( -32.01814843081346851, 533.1823905683720568, -16.75240474999999307 ) ) ;
#5083 = CARTESIAN_POINT ( 'NONE',  ( -24.70764059509554045, 300.0573905601784759, 19.99999999999998934 ) ) ;
#5084 = DIRECTION ( 'NONE',  ( -1.000000000000000000, -0.000000000000000000, -0.000000000000000000 ) ) ;
#5085 = CARTESIAN_POINT ( 'NONE',  ( -11.93348319268872260, 340.0573905683720568, 3.332260488124728859 ) ) ;
#5086 = ORIENTED_EDGE ( 'NONE', *, *, #6536, .F. ) ;
#5087 = CARTESIAN_POINT ( 'NONE',  ( -24.70764059509557597, 479.1823905765656377, -19.99999999999999289 ) ) ;
#5088 = CARTESIAN_POINT ( 'NONE',  ( -11.93348319268872260, 358.5573905683720000, 3.332260488124728415 ) ) ;
#5089 = CARTESIAN_POINT ( 'NONE',  ( -44.16309181155856578, 364.4948905683720568, 6.410867750099241924 ) ) ;
#5090 = VECTOR ( 'NONE', #2953, 1000.000000000000000 ) ;
#5091 = CARTESIAN_POINT ( 'NONE',  ( -40.01497788969912506, 313.5573905765655809, 16.95518130045146776 ) ) ;
#5092 = FACE_OUTER_BOUND ( 'NONE', #10821, .T. ) ;
#5093 = CARTESIAN_POINT ( 'NONE',  ( -11.93348319268871016, 269.1823905683720000, -3.332260488124732856 ) ) ;
#5094 = FACE_OUTER_BOUND ( 'NONE', #5448, .T. ) ;
#5095 = CARTESIAN_POINT ( 'NONE',  ( -19.19641293061499354, 441.9323905683720568, -14.20200298773971603 ) ) ;
#5096 = DIRECTION ( 'NONE',  ( -0.000000000000000000, -1.000000000000000000, -0.000000000000000000 ) ) ;
#5097 = DIRECTION ( 'NONE',  ( -0.000000000000000000, -0.000000000000000000, -1.000000000000000000 ) ) ;
#5098 = DIRECTION ( 'NONE',  ( -1.191790137725560488E-16, 1.000000000000000000, -0.000000000000000000 ) ) ;
#5099 = PRODUCT_DEFINITION_CONTEXT ( 'detailed design', #20777, 'design' ) ;
#5100 = CARTESIAN_POINT ( 'NONE',  ( -28.68588794268875120, 585.7448905601785327, 0.000000000000000000 ) ) ;
#5101 = CARTESIAN_POINT ( 'NONE',  ( -11.93348319268872260, 340.0573905683720000, 3.332260488124728415 ) ) ;
#5102 = CARTESIAN_POINT ( 'NONE',  ( -14.48388495494901385, 479.8073905683720568, -9.489475012073736337 ) ) ;
#5103 = VERTEX_POINT ( 'NONE', #9002 ) ;
#5104 = CARTESIAN_POINT ( 'NONE',  ( -24.70764059509557597, 484.4323905601785327, -19.99999999999999289 ) ) ;
#5105 = CARTESIAN_POINT ( 'NONE',  ( -22.27502019258946930, 296.9948905683720000, 15.47720386886985189 ) ) ;
#5106 = ORIENTED_EDGE ( 'NONE', *, *, #13678, .T. ) ;
#5107 = CARTESIAN_POINT ( 'NONE',  ( -47.16347859291444422, 342.6198905765656377, 7.653668647301805628 ) ) ;
#5108 = VERTEX_POINT ( 'NONE', #5754 ) ;
#5109 = DIRECTION ( 'NONE',  ( 0.000000000000000000, 1.000000000000000000, 0.000000000000000000 ) ) ;
#5110 = EDGE_CURVE ( 'NONE', #6162, #4291, #1425, .T. ) ;
#5111 = CARTESIAN_POINT ( 'NONE',  ( -11.93348319268872615, 400.0573905683720568, 3.332260488124728859 ) ) ;
#5112 = CARTESIAN_POINT ( 'NONE',  ( -32.66413529028188378, 479.4323905601785327, 19.99999999999999289 ) ) ;
#5113 = CARTESIAN_POINT ( 'NONE',  ( -14.54375231895776999, 385.7448905765656377, 14.14213562373094568 ) ) ;
#5114 = CARTESIAN_POINT ( 'NONE',  ( -40.53162694259544452, 415.1198905683720000, 11.84573899990672885 ) ) ;
#5115 = CARTESIAN_POINT ( 'NONE',  ( -13.20868407381884779, 269.7448905683720568, 6.410867750099229490 ) ) ;
#5116 = CARTESIAN_POINT ( 'NONE',  ( -22.27502019258948707, 436.9948905683720568, 15.47720386886985189 ) ) ;
#5117 = DIRECTION ( 'NONE',  ( 0.000000000000000000, 0.000000000000000000, 1.000000000000000000 ) ) ;
#5118 = CARTESIAN_POINT ( 'NONE',  ( -14.54375231895777176, 400.9948905601785327, 14.14213562373094568 ) ) ;
#5119 = CARTESIAN_POINT ( 'NONE',  ( -14.54375231895776643, 355.7448905765655809, 14.14213562373094568 ) ) ;
#5120 = FACE_OUTER_BOUND ( 'NONE', #14147, .T. ) ;
#5121 = CARTESIAN_POINT ( 'NONE',  ( -36.33955658999051508, 390.1198905765656377, -18.47759065022572855 ) ) ;
#5122 = CARTESIAN_POINT ( 'NONE',  ( -42.88789093042843348, 332.9323905683719431, -9.489475012073734561 ) ) ;
#5123 = CARTESIAN_POINT ( 'NONE',  ( -28.68588794268873343, 489.4948905765656377, -19.99999999999999289 ) ) ;
#5124 = CARTESIAN_POINT ( 'NONE',  ( -25.35362745456399836, 498.1823905683720000, 16.75240474999998952 ) ) ;
#5125 = EDGE_CURVE ( 'NONE', #17724, #2963, #4569, .T. ) ;
#5126 = CARTESIAN_POINT ( 'NONE',  ( -162.2727221670389781, 10.52886280891152104, 20.57735571454641033 ) ) ;
#5127 = CARTESIAN_POINT ( 'NONE',  ( -24.70764059509556887, 464.4323905601784190, -19.99999999999999289 ) ) ;
#5128 = DIRECTION ( 'NONE',  ( -1.191790137725560488E-16, 1.000000000000000000, -0.000000000000000000 ) ) ;
#5129 = EDGE_CURVE ( 'NONE', #16429, #15603, #15940, .T. ) ;
#5130 = EDGE_CURVE ( 'NONE', #1471, #2121, #1228, .T. ) ;
#5131 = CARTESIAN_POINT ( 'NONE',  ( -45.43829269268871229, 405.0573905683721136, -3.332260488124726194 ) ) ;
#5132 = FACE_OUTER_BOUND ( 'NONE', #10074, .T. ) ;
#5133 = CARTESIAN_POINT ( 'NONE',  ( -14.48388495494898365, 239.4323905683720000, 9.489475012073732785 ) ) ;
#5134 = CARTESIAN_POINT ( 'NONE',  ( -38.17536295476244845, 365.4323905683720000, 14.20200298773971781 ) ) ;
#5135 = AXIS2_PLACEMENT_3D ( 'NONE', #4764, #2841, #4663 ) ;
#5136 = ORIENTED_EDGE ( 'NONE', *, *, #19094, .F. ) ;
#5137 = CARTESIAN_POINT ( 'NONE',  ( -25.35362745456400191, 526.6823905683720568, 16.75240474999998952 ) ) ;
#5138 = ORIENTED_EDGE ( 'NONE', *, *, #10446, .T. ) ;
#5139 = CARTESIAN_POINT ( 'NONE',  ( -32.01814843081344719, 447.5573905683720000, 16.75240474999999307 ) ) ;
#5140 = CARTESIAN_POINT ( 'NONE',  ( -28.68588794268873698, 521.3698905683720568, -16.75240474999999307 ) ) ;
#5141 = EDGE_CURVE ( 'NONE', #11401, #7492, #3055, .T. ) ;
#5142 = ORIENTED_EDGE ( 'NONE', *, *, #15447, .F. ) ;
#5143 = CARTESIAN_POINT ( 'NONE',  ( -48.68588794268871567, 427.2448905601784759, 0.000000000000000000 ) ) ;
#5144 = CARTESIAN_POINT ( 'NONE',  ( -19.19641293061499354, 487.3073905683719431, 14.20200298773971426 ) ) ;
#5145 = ORIENTED_EDGE ( 'NONE', *, *, #4677, .T. ) ;
#5146 = CARTESIAN_POINT ( 'NONE',  ( -19.19641293061500065, 500.4323905683720568, -14.20200298773971603 ) ) ;
#5147 = CARTESIAN_POINT ( 'NONE',  ( -12.15536544594166557, 51.34507591104713953, -46.76614217995071954 ) ) ;
#5148 = CARTESIAN_POINT ( 'NONE',  ( -36.33955658999052218, 423.8698905765655809, 18.47759065022572500 ) ) ;
#5149 = DIRECTION ( 'NONE',  ( -0.000000000000000000, -0.000000000000000000, -1.000000000000000000 ) ) ;
#5150 = CARTESIAN_POINT ( 'NONE',  ( -18.68588794268873698, 281.1055109169419666, -20.00000000000000355 ) ) ;
#5151 = FACE_OUTER_BOUND ( 'NONE', #3444, .T. ) ;
#5152 = DIRECTION ( 'NONE',  ( 1.000000000000000000, -0.000000000000000000, 0.000000000000000000 ) ) ;
#5153 = DIRECTION ( 'NONE',  ( 1.000000000000000000, -0.000000000000000000, -0.000000000000000000 ) ) ;
#5154 = CIRCLE ( 'NONE', #13448, 15.00000000000000000 ) ;
#5155 = CARTESIAN_POINT ( 'NONE',  ( -12.23124753831989509, 223.9102039777117739, -11.50152087354334007 ) ) ;
#5156 =( BOUNDED_CURVE ( )  B_SPLINE_CURVE ( 2, ( #18642, #5245, #11845, #5031, #10422, #18442, #5346, #17044, #2225, #14895, #16833, #3728, #10313, #3941, #17457, #10853, #15531 ),
 .UNSPECIFIED., .F., .T. ) 
 B_SPLINE_CURVE_WITH_KNOTS ( ( 3, 2, 2, 2, 2, 2, 2, 2, 3 ),
 ( 0.1250000000000001110, 0.1269531250000001110, 0.1289062500000001110, 0.1308593750000001110, 0.1328125000000001110, 0.1347656250000001388, 0.1367187500000001388, 0.1386718750000001388, 0.1406250000000001388 ),
 .UNSPECIFIED. ) 
 CURVE ( )  GEOMETRIC_REPRESENTATION_ITEM ( )  RATIONAL_B_SPLINE_CURVE ( ( 0.9999999999999988898, 0.9807852804032315408, 1.000000000000000000, 0.9807852804032304306, 1.000000000000000000, 0.9807852804032304306, 1.000000000000000000, 0.9807852804032304306, 1.000000000000000000, 0.9807852804032304306, 1.000000000000000000, 0.9807852804032304306, 1.000000000000000000, 0.9807852804032304306, 1.000000000000000000, 0.9807852804032290983, 1.000000000000001332 ) ) 
 REPRESENTATION_ITEM ( '' )  );
#5157 = CARTESIAN_POINT ( 'NONE',  ( -22.27502019258947996, 292.2448905683720000, -15.47720386886985544 ) ) ;
#5158 = DIRECTION ( 'NONE',  ( -1.000000000000000000, -0.000000000000000000, -0.000000000000000000 ) ) ;
#5159 = CARTESIAN_POINT ( 'NONE',  ( -40.01497788969913216, 275.6823905601784759, -16.95518130045146421 ) ) ;
#5160 = CARTESIAN_POINT ( 'NONE',  ( 88.28695088269886071, 152.5259582928263740, 20.00000000000000355 ) ) ;
#5161 = CARTESIAN_POINT ( 'NONE',  ( -22.27502019258947641, 282.2448905683720568, -15.47720386886985544 ) ) ;
#5162 = ORIENTED_EDGE ( 'NONE', *, *, #300, .F. ) ;
#5163 = LINE ( 'NONE', #16752, #11180 ) ;
#5164 = CARTESIAN_POINT ( 'NONE',  ( -19.19641293061500065, 501.9323905683720000, -14.20200298773971603 ) ) ;
#5165 = VECTOR ( 'NONE', #11667, 1000.000000000000000 ) ;
#5166 = EDGE_LOOP ( 'NONE', ( #16934, #15317 ) ) ;
#5167 = CARTESIAN_POINT ( 'NONE',  ( -16.84014894278200103, 461.6198905683720568, -11.84573899990672707 ) ) ;
#5168 = CARTESIAN_POINT ( 'NONE',  ( -21.03221929538693047, 408.8698905765656377, -18.47759065022572855 ) ) ;
#5169 = CARTESIAN_POINT ( 'NONE',  ( -19.19641293061497578, 260.4323905683720000, -14.20200298773971603 ) ) ;
#5170 = VERTEX_POINT ( 'NONE', #9322 ) ;
#5171 = CARTESIAN_POINT ( 'NONE',  ( 0.4037800551813805483, -7.199367570657614124, -0.5303295852573159941 ) ) ;
#5172 = CARTESIAN_POINT ( 'NONE',  ( -14.48388495494898542, 251.3073905683720284, -9.489475012073734561 ) ) ;
#5173 = CARTESIAN_POINT ( 'NONE',  ( -42.82802356641964536, 250.7448905765656377, -14.14213562373094746 ) ) ;
#5174 = DIRECTION ( 'NONE',  ( -0.000000000000000000, -1.000000000000000000, -0.000000000000000000 ) ) ;
#5175 = CARTESIAN_POINT ( 'NONE',  ( -8.685887942688706786, 231.9323905601785043, 3.978247347593161010 ) ) ;
#5176 = CARTESIAN_POINT ( 'NONE',  ( -44.16309181155855157, 264.4948905683720000, 6.410867750099241924 ) ) ;
#5177 = CARTESIAN_POINT ( 'NONE',  ( -13.20868407381885845, 359.7448905683720568, 6.410867750099229490 ) ) ;
#5178 = EDGE_CURVE ( 'NONE', #20702, #15032, #10839, .T. ) ;
#5179 = CARTESIAN_POINT ( 'NONE',  ( -40.01497788969915348, 505.6823905601784759, -16.95518130045146421 ) ) ;
#5180 = DIRECTION ( 'NONE',  ( -1.000000000000000000, 0.000000000000000000, -0.000000000000000000 ) ) ;
#5181 = B_SPLINE_CURVE_WITH_KNOTS ( 'NONE', 3,
 ( #20087, #18555, #9904, #16525, #5257, #8277 ),
 .UNSPECIFIED., .F., .F.,
 ( 4, 2, 4 ),
 ( 0.02294124189192014301, 0.02484059228024679267, 0.02673994266857344232 ),
 .UNSPECIFIED. ) ;
#5182 = DIRECTION ( 'NONE',  ( 0.000000000000000000, -0.5000000000000011102, -0.8660254037844380415 ) ) ;
#5183 = ORIENTED_EDGE ( 'NONE', *, *, #16038, .F. ) ;
#5184 = AXIS2_PLACEMENT_3D ( 'NONE', #1348, #7921, #21135 ) ;
#5185 = CARTESIAN_POINT ( 'NONE',  ( -21.03221929538692692, 404.1198905601784759, -18.47759065022572855 ) ) ;
#5186 = EDGE_LOOP ( 'NONE', ( #7249, #19963, #5241, #14308 ) ) ;
#5187 = ORIENTED_EDGE ( 'NONE', *, *, #5192, .T. ) ;
#5188 = ORIENTED_EDGE ( 'NONE', *, *, #18160, .F. ) ;
#5189 = CARTESIAN_POINT ( 'NONE',  ( -44.16309181155858710, 525.9948905683720568, 6.410867750099241924 ) ) ;
#5190 = CARTESIAN_POINT ( 'NONE',  ( -14.54375231895775755, 290.9948905601784759, 14.14213562373094568 ) ) ;
#5191 = CARTESIAN_POINT ( 'NONE',  ( -42.99906419454242013, 207.3703986995724335, -4.488953568700487118 ) ) ;
#5192 = EDGE_CURVE ( 'NONE', #8982, #1338, #2633, .T. ) ;
#5193 = CARTESIAN_POINT ( 'NONE',  ( -14.48388495494899253, 319.4323905683720000, 9.489475012073731008 ) ) ;
#5194 = CARTESIAN_POINT ( 'NONE',  ( -22.27502019258948707, 360.7448905683720568, -15.47720386886985544 ) ) ;
#5195 = CARTESIAN_POINT ( 'NONE',  ( -19.19641293061497933, 367.3073905683720000, 14.20200298773971426 ) ) ;
#5196 = CARTESIAN_POINT ( 'NONE',  ( -8.685887942688715668, 296.6823905765655809, 3.978247347593161010 ) ) ;
#5197 = DIRECTION ( 'NONE',  ( 0.000000000000000000, 0.000000000000000000, 1.000000000000000000 ) ) ;
#5198 = CARTESIAN_POINT ( 'NONE',  ( -11.93348319268871016, 268.5573905683720000, 3.332260488124728859 ) ) ;
#5199 = CARTESIAN_POINT ( 'NONE',  ( -45.64106924314018698, 438.1823905601784190, 11.32908994701042538 ) ) ;
#5200 = CLOSED_SHELL ( 'NONE', ( #2456, #16599, #10713, #4274, #15176, #4484, #20468, #7353, #10531, #6510, #18478, #8194, #18073, #13463, #16844, #14313, #1146, #5645, #15991, #2247, #2026, #3612, #11674, #9859, #8507, #14682, #9340, #6652, #18819, #3857, #4641, #16723, #7685, #18075 ) ) ;
#5201 = CARTESIAN_POINT ( 'NONE',  ( -11.93348319268872793, 420.6823905683720000, -3.332260488124732856 ) ) ;
#5202 = EDGE_CURVE ( 'NONE', #10415, #10685, #21013, .T. ) ;
#5203 = DIRECTION ( 'NONE',  ( -0.000000000000000000, -1.000000000000000000, -0.000000000000000000 ) ) ;
#5204 = CARTESIAN_POINT ( 'NONE',  ( -21.03221929538694113, 514.1198905601785327, -18.47759065022572855 ) ) ;
#5205 = DIRECTION ( 'NONE',  ( 0.000000000000000000, -0.5000000000000018874, -0.8660254037844374864 ) ) ;
#5206 = CARTESIAN_POINT ( 'NONE',  ( -45.64106924314018698, 408.1823905601784759, 11.32908994701042538 ) ) ;
#5207 = CARTESIAN_POINT ( 'NONE',  ( -25.35362745456398770, 332.5573905683720000, -16.75240474999999307 ) ) ;
#5208 = CARTESIAN_POINT ( 'NONE',  ( -25.35362745456399480, 476.6823905683720000, 16.75240474999998952 ) ) ;
#5209 = VERTEX_POINT ( 'NONE', #4671 ) ;
#5210 = CARTESIAN_POINT ( 'NONE',  ( -10.20829729246299777, 461.6198905601784759, 7.653668647301790529 ) ) ;
#5211 = CARTESIAN_POINT ( 'NONE',  ( -25.35362745456398414, 311.0573905683720568, -16.75240474999999307 ) ) ;
#5212 = AXIS2_PLACEMENT_3D ( 'NONE', #18871, #13809, #18983 ) ;
#5213 = AXIS2_PLACEMENT_3D ( 'NONE', #21198, #5180, #11776 ) ;
#5214 = CARTESIAN_POINT ( 'NONE',  ( 0.01372220897661846455, -5.309964801958114933, 3.802871176606136050 ) ) ;
#5215 = ORIENTED_EDGE ( 'NONE', *, *, #250, .T. ) ;
#5216 = LINE ( 'NONE', #8561, #10162 ) ;
#5217 = CARTESIAN_POINT ( 'NONE',  ( -22.27502019258949062, 382.2448905683720000, -15.47720386886985544 ) ) ;
#5218 = CARTESIAN_POINT ( 'NONE',  ( -21.03221929538692336, 480.3698905601784759, 18.47759065022572500 ) ) ;
#5219 = DIRECTION ( 'NONE',  ( 0.000000000000000000, -1.000000000000000000, 0.000000000000000000 ) ) ;
#5220 = CARTESIAN_POINT ( 'NONE',  ( -11.93348319268872970, 429.1823905683720568, -3.332260488124732856 ) ) ;
#5221 = CARTESIAN_POINT ( 'NONE',  ( -28.68588794268870146, 267.8698905683720000, 16.75240474999999307 ) ) ;
#5222 = AXIS2_PLACEMENT_3D ( 'NONE', #14316, #2838, #9420 ) ;
#5223 = CARTESIAN_POINT ( 'NONE',  ( -45.43829269268871940, 433.5573905683719431, -3.332260488124726638 ) ) ;
#5224 =( LENGTH_UNIT ( ) NAMED_UNIT ( * ) SI_UNIT ( .MILLI., .METRE. ) );
#5225 = FACE_OUTER_BOUND ( 'NONE', #10918, .T. ) ;
#5226 = CARTESIAN_POINT ( 'NONE',  ( -10.20829729246298534, 357.6198905765656377, -7.653668647301794969 ) ) ;
#5227 = CARTESIAN_POINT ( 'NONE',  ( -32.66413529028185536, 275.0573905601784759, -19.99999999999999289 ) ) ;
#5228 = CARTESIAN_POINT ( 'NONE',  ( -8.685887942688726326, 386.9948905765655809, -2.449293598294705724E-15 ) ) ;
#5229 = CARTESIAN_POINT ( 'NONE',  ( -28.68588794268870856, 326.3698905683720000, 16.75240474999999307 ) ) ;
#5230 = LINE ( 'NONE', #3505, #8285 ) ;
#5231 = CARTESIAN_POINT ( 'NONE',  ( -25.35362745456400546, 472.5573905683720568, -16.75240474999999307 ) ) ;
#5232 = CARTESIAN_POINT ( 'NONE',  ( -28.68588794268875475, 600.7448905601785327, 0.000000000000000000 ) ) ;
#5233 = SURFACE_STYLE_FILL_AREA ( #8140 ) ;
#5234 = CARTESIAN_POINT ( 'NONE',  ( -42.82802356641966668, 418.4948905601784759, 14.14213562373094923 ) ) ;
#5235 = CARTESIAN_POINT ( 'NONE',  ( -44.16309181155857289, 384.7448905683720000, -6.410867750099231266 ) ) ;
#5236 = DIRECTION ( 'NONE',  ( 0.000000000000000000, 0.000000000000000000, 1.000000000000000000 ) ) ;
#5237 = CARTESIAN_POINT ( 'NONE',  ( -14.48388495494898365, 231.3073905683720000, -9.489475012073736337 ) ) ;
#5238 = CARTESIAN_POINT ( 'NONE',  ( -14.48388495494899786, 357.9323905683720568, 9.489475012073732785 ) ) ;
#5239 = ORIENTED_EDGE ( 'NONE', *, *, #1041, .T. ) ;
#5240 = CARTESIAN_POINT ( 'NONE',  ( -16.84014894278200458, 517.6198905683719431, 11.84573899990672530 ) ) ;
#5241 = ORIENTED_EDGE ( 'NONE', *, *, #401, .T. ) ;
#5242 = CARTESIAN_POINT ( 'NONE',  ( -14.48388495494900852, 449.4323905683721705, 9.489475012073731008 ) ) ;
#5243 = CARTESIAN_POINT ( 'NONE',  ( -32.01814843081346851, 516.0573905683720568, 16.75240474999999307 ) ) ;
#5244 = VERTEX_POINT ( 'NONE', #10941 ) ;
#5245 = CARTESIAN_POINT ( 'NONE',  ( -48.68588794268863040, 496.9323905601785327, -3.978247347593371508 ) ) ;
#5246 = CARTESIAN_POINT ( 'NONE',  ( -44.16309181155858710, 493.2448905683720000, -6.410867750099231266 ) ) ;
#5247 = EDGE_CURVE ( 'NONE', #7551, #9807, #19708, .T. ) ;
#5248 = AXIS2_PLACEMENT_3D ( 'NONE', #16418, #10994, #3110 ) ;
#5249 = EDGE_LOOP ( 'NONE', ( #14465, #11892, #11024, #7834, #10874, #11376 ) ) ;
#5250 = CARTESIAN_POINT ( 'NONE',  ( -38.17536295476246977, 492.3073905683720000, -14.20200298773971426 ) ) ;
#5251 = CARTESIAN_POINT ( 'NONE',  ( -21.03221929538692336, 490.3698905601784759, 18.47759065022572500 ) ) ;
#5252 = CARTESIAN_POINT ( 'NONE',  ( -48.68588794268871567, 421.6823905765655809, -3.978247347593158345 ) ) ;
#5253 = CARTESIAN_POINT ( 'NONE',  ( 65.85920792673738333, 160.1716627696692683, -40.00000000000000000 ) ) ;
#5254 = DIRECTION ( 'NONE',  ( 0.000000000000000000, 0.000000000000000000, -1.000000000000000000 ) ) ;
#5255 = CARTESIAN_POINT ( 'NONE',  ( -28.68588794268872988, 484.7448905601784759, -19.99999999999999289 ) ) ;
#5256 = CARTESIAN_POINT ( 'NONE',  ( -28.68588794268875120, 585.7448905601785327, 0.000000000000000000 ) ) ;
#5257 = CARTESIAN_POINT ( 'NONE',  ( 0.4042117618287694447, -3.141900367811087502, -6.500000000000000000 ) ) ;
#5258 = CARTESIAN_POINT ( 'NONE',  ( -8.685887942688969687, 496.6823905765655240, 3.978247347593719230 ) ) ;
#5259 = CARTESIAN_POINT ( 'NONE',  ( -13.20868407381885135, 299.7448905683720568, 6.410867750099229490 ) ) ;
#5260 = EDGE_CURVE ( 'NONE', #454, #4584, #18341, .T. ) ;
#5261 = CARTESIAN_POINT ( 'NONE',  ( -48.68588794268873698, 573.2448905601785327, 0.000000000000000000 ) ) ;
#5262 = CARTESIAN_POINT ( 'NONE',  ( -45.43829269268871940, 455.0573905683720568, -3.332260488124726194 ) ) ;
#5263 = CARTESIAN_POINT ( 'NONE',  ( -36.33955658999052218, 413.8698905765655809, 18.47759065022572500 ) ) ;
#5264 = CIRCLE ( 'NONE', #13574, 10.00000000000000888 ) ;
#5265 = ORIENTED_EDGE ( 'NONE', *, *, #5077, .T. ) ;
#5266 = CARTESIAN_POINT ( 'NONE',  ( -45.43829269268872650, 495.3698905683720568, 0.000000000000000000 ) ) ;
#5267 = VERTEX_POINT ( 'NONE', #2741 ) ;
#5268 = CARTESIAN_POINT ( 'NONE',  ( -11.93348319268873503, 470.3698905683720568, -2.051577885510841163E-15 ) ) ;
#5269 = DIRECTION ( 'NONE',  ( -1.191790137725560488E-16, 1.000000000000000000, -0.000000000000000000 ) ) ;
#5270 = CARTESIAN_POINT ( 'NONE',  ( -38.17536295476244135, 262.3073905683720568, -14.20200298773971426 ) ) ;
#5271 = AXIS2_PLACEMENT_3D ( 'NONE', #14027, #4160, #7507 ) ;
#5272 = VERTEX_POINT ( 'NONE', #11159 ) ;
#5273 = CARTESIAN_POINT ( 'NONE',  ( -32.66413529028186957, 334.1823905765656946, 19.99999999999999289 ) ) ;
#5274 = CARTESIAN_POINT ( 'NONE',  ( -42.88789093042841927, 246.3073905683720284, 9.489475012073734561 ) ) ;
#5275 = CARTESIAN_POINT ( 'NONE',  ( 105.7989814974898479, 142.5259582928263455, 40.00000000000000000 ) ) ;
#5276 = CYLINDRICAL_SURFACE ( 'NONE', #4232, 9.999999999999994671 ) ;
#5277 = AXIS2_PLACEMENT_3D ( 'NONE', #20158, #5326, #10086 ) ;
#5278 = CARTESIAN_POINT ( 'NONE',  ( -40.53162694259542320, 262.6198905683720568, -11.84573899990672707 ) ) ;
#5279 = CARTESIAN_POINT ( 'NONE',  ( -44.16309181155856578, 355.9948905683720000, 6.410867750099241924 ) ) ;
#5280 = CARTESIAN_POINT ( 'NONE',  ( -8.685887942688738761, 502.2448905601784190, -2.449293598294705724E-15 ) ) ;
#5281 = AXIS2_PLACEMENT_3D ( 'NONE', #6580, #9822, #7878 ) ;
#5282 = CARTESIAN_POINT ( 'NONE',  ( -35.09675569278795138, 411.9948905683720000, -15.47720386886985544 ) ) ;
#5283 = CARTESIAN_POINT ( 'NONE',  ( -21.03221929538692692, 510.3698905601785896, 18.47759065022572500 ) ) ;
#5284 = ORIENTED_EDGE ( 'NONE', *, *, #5335, .F. ) ;
#5285 = CARTESIAN_POINT ( 'NONE',  ( -14.54375231895777176, 400.9948905601785327, 14.14213562373094568 ) ) ;
#5286 = ORIENTED_EDGE ( 'NONE', *, *, #2140, .F. ) ;
#5287 = CARTESIAN_POINT ( 'NONE',  ( -1.025382690249031503, 230.5765313837437418, 25.00000000000000000 ) ) ;
#5288 = VERTEX_POINT ( 'NONE', #14641 ) ;
#5289 = ORIENTED_EDGE ( 'NONE', *, *, #18674, .F. ) ;
#5290 = CARTESIAN_POINT ( 'NONE',  ( -22.27502019258950483, 522.2448905683720568, -15.47720386886985544 ) ) ;
#5291 = CARTESIAN_POINT ( 'NONE',  ( -28.68588794268870146, 289.7448905601784759, 19.99999999999999289 ) ) ;
#5292 = AXIS2_PLACEMENT_3D ( 'NONE', #4209, #444, #18585 ) ;
#5293 = CARTESIAN_POINT ( 'NONE',  ( -11.93348319268871549, 320.0573905683720000, 3.332260488124728859 ) ) ;
#5294 = ORIENTED_EDGE ( 'NONE', *, *, #13678, .F. ) ;
#5295 = CARTESIAN_POINT ( 'NONE',  ( -40.53162694259543741, 355.1198905683720568, 11.84573899990672885 ) ) ;
#5296 = VECTOR ( 'NONE', #9079, 1000.000000000000000 ) ;
#5297 = CARTESIAN_POINT ( 'NONE',  ( -11.93348319268872260, 358.5573905683720000, 3.332260488124728859 ) ) ;
#5298 = CARTESIAN_POINT ( 'NONE',  ( -48.68588794268870146, 312.3073905765655809, 3.978247347593168115 ) ) ;
#5299 = DIRECTION ( 'NONE',  ( -0.000000000000000000, -0.000000000000000000, -1.000000000000000000 ) ) ;
#5300 = EDGE_CURVE ( 'NONE', #14361, #10309, #14710, .T. ) ;
#5301 = CARTESIAN_POINT ( 'NONE',  ( -25.35362745456398059, 261.0573905683720000, -16.75240474999999307 ) ) ;
#5302 = CARTESIAN_POINT ( 'NONE',  ( -32.66413529028187668, 439.4323905601785327, 19.99999999999999289 ) ) ;
#5303 = CARTESIAN_POINT ( 'NONE',  ( -25.35362745456399836, 422.5573905683721136, -16.75240474999999307 ) ) ;
#5304 = CARTESIAN_POINT ( 'NONE',  ( -48.68588794268873698, 573.2448905601785327, 0.000000000000000000 ) ) ;
#5305 = CARTESIAN_POINT ( 'NONE',  ( -8.685887942688720997, 352.2448905601784759, -2.449293598294705724E-15 ) ) ;
#5306 = CARTESIAN_POINT ( 'NONE',  ( -8.685887942688893304, 306.6823905765655240, 3.978247347593586447 ) ) ;
#5307 = CARTESIAN_POINT ( 'NONE',  ( -11.73070664223724968, 411.3073905601784759, 11.32908994701042005 ) ) ;
#5308 = CARTESIAN_POINT ( 'NONE',  ( -13.20868407381885667, 330.9948905683720000, -6.410867750099233042 ) ) ;
#5309 = CARTESIAN_POINT ( 'NONE',  ( -32.01814843081346140, 456.0573905683720000, 16.75240474999999307 ) ) ;
#5310 = ORIENTED_EDGE ( 'NONE', *, *, #6130, .T. ) ;
#5311 = CARTESIAN_POINT ( 'NONE',  ( -48.68588794268872277, 457.5573905601784190, 3.978247347593168115 ) ) ;
#5312 = CARTESIAN_POINT ( 'NONE',  ( -13.20868407381885490, 309.4948905683720568, -6.410867750099233042 ) ) ;
#5313 = AXIS2_PLACEMENT_3D ( 'NONE', #17739, #9511, #19468 ) ;
#5314 = CARTESIAN_POINT ( 'NONE',  ( -8.685887942688898633, 341.9323905601785327, 3.978247347593586447 ) ) ;
#5315 = ORIENTED_EDGE ( 'NONE', *, *, #18995, .T. ) ;
#5316 = DIRECTION ( 'NONE',  ( -1.000000000000000000, 0.000000000000000000, 0.000000000000000000 ) ) ;
#5317 = CARTESIAN_POINT ( 'NONE',  ( -11.73070664223724613, 341.3073905601785327, 11.32908994701042005 ) ) ;
#5318 = EDGE_CURVE ( 'NONE', #14150, #10771, #4173, .T. ) ;
#5319 = CARTESIAN_POINT ( 'NONE',  ( -14.48388495494900141, 389.4323905683720568, 9.489475012073731008 ) ) ;
#5320 = CARTESIAN_POINT ( 'NONE',  ( -48.68588794268854514, 376.9323905601785327, -3.978247347593583783 ) ) ;
#5321 = DIRECTION ( 'NONE',  ( -0.000000000000000000, -0.000000000000000000, -1.000000000000000000 ) ) ;
#5322 = CARTESIAN_POINT ( 'NONE',  ( -42.88789093042844058, 422.9323905683720000, -9.489475012073736337 ) ) ;
#5323 = CARTESIAN_POINT ( 'NONE',  ( -42.88789093042841927, 266.3073905683720000, 9.489475012073736337 ) ) ;
#5324 = CARTESIAN_POINT ( 'NONE',  ( -32.01814843081344719, 421.6823905683720568, -16.75240474999999307 ) ) ;
#5325 = PRODUCT_CONTEXT ( 'NONE', #1706, 'mechanical' ) ;
#5326 = DIRECTION ( 'NONE',  ( 0.000000000000000000, 1.000000000000000000, 0.000000000000000000 ) ) ;
#5327 = CARTESIAN_POINT ( 'NONE',  ( -42.82802356641965957, 373.2448905765656377, 14.14213562373094923 ) ) ;
#5328 = DIRECTION ( 'NONE',  ( -1.000000000000000000, 0.000000000000000000, 0.000000000000000000 ) ) ;
#5329 = CARTESIAN_POINT ( 'NONE',  ( -40.53162694259543031, 322.6198905683720568, -11.84573899990672707 ) ) ;
#5330 = CARTESIAN_POINT ( 'NONE',  ( -45.64106924314019409, 491.0573905765656377, -11.32908994701042538 ) ) ;
#5331 = CARTESIAN_POINT ( 'NONE',  ( -11.93348319268873503, 480.0573905683720568, 3.332260488124728415 ) ) ;
#5332 = CARTESIAN_POINT ( 'NONE',  ( -28.68588794268872277, 434.4948905765655809, 19.99999999999999289 ) ) ;
#5333 = CARTESIAN_POINT ( 'NONE',  ( 0.000000000000000000, -5.629165124598849879, -3.250000000000003553 ) ) ;
#5334 = PLANE ( 'NONE',  #14404 ) ;
#5335 = EDGE_CURVE ( 'NONE', #20381, #11578, #1023, .T. ) ;
#5336 = CARTESIAN_POINT ( 'NONE',  ( -44.16309181155857999, 394.7448905683720568, -6.410867750099231266 ) ) ;
#5337 = DIRECTION ( 'NONE',  ( 1.000000000000000000, 0.000000000000000000, 0.000000000000000000 ) ) ;
#5338 = CARTESIAN_POINT ( 'NONE',  ( -11.73070664223726567, 521.3073905601785327, 11.32908994701042005 ) ) ;
#5339 = CARTESIAN_POINT ( 'NONE',  ( -19.19641293061498288, 367.3073905683720000, 14.20200298773971426 ) ) ;
#5340 = ORIENTED_EDGE ( 'NONE', *, *, #992, .F. ) ;
#5341 = CARTESIAN_POINT ( 'NONE',  ( -19.19641293061500420, 520.4323905683720568, -14.20200298773971603 ) ) ;
#5342 = VERTEX_POINT ( 'NONE', #5973 ) ;
#5343 = CARTESIAN_POINT ( 'NONE',  ( -44.16309181155859420, 523.2448905683719431, -6.410867750099231266 ) ) ;
#5344 = EDGE_CURVE ( 'NONE', #20997, #11679, #2110, .T. ) ;
#5345 = ORIENTED_EDGE ( 'NONE', *, *, #4201, .T. ) ;
#5346 = CARTESIAN_POINT ( 'NONE',  ( -36.33955658999052218, 495.3698905601784759, -18.47759065022572855 ) ) ;
#5347 = CARTESIAN_POINT ( 'NONE',  ( -16.84014894278200103, 477.6198905683720000, 11.84573899990672530 ) ) ;
#5348 = EDGE_LOOP ( 'NONE', ( #1856, #19473 ) ) ;
#5349 = CARTESIAN_POINT ( 'NONE',  ( -44.16309181155858710, 483.2448905683720000, -6.410867750099231266 ) ) ;
#5350 = CARTESIAN_POINT ( 'NONE',  ( -47.16347859291445843, 487.8698905601784759, 7.653668647301805628 ) ) ;
#5351 = CARTESIAN_POINT ( 'NONE',  ( -11.73070664223725679, 417.9323905765656377, -11.32908994701042715 ) ) ;
#5352 = PLANE ( 'NONE',  #9632 ) ;
#5353 = CYLINDRICAL_SURFACE ( 'NONE', #14088, 5.000000000000004441 ) ;
#5354 = CARTESIAN_POINT ( 'NONE',  ( -45.64106924314019409, 486.3073905601785327, -11.32908994701042538 ) ) ;
#5355 = CARTESIAN_POINT ( 'NONE',  ( 82.89408817951444064, 286.0648460576640559, -40.00000000000000000 ) ) ;
#5356 = CARTESIAN_POINT ( 'NONE',  ( 115.7989814974898337, 142.5259582928263455, 40.00000000000000000 ) ) ;
#5357 = LINE ( 'NONE', #10327, #18685 ) ;
#5358 = CARTESIAN_POINT ( 'NONE',  ( -35.09675569278794427, 297.2448905683720000, 15.47720386886985366 ) ) ;
#5359 = CARTESIAN_POINT ( 'NONE',  ( -8.685887942688616192, 232.5573905601784759, -3.978247347592952732 ) ) ;
#5360 = CARTESIAN_POINT ( 'NONE',  ( -11.93348319268873148, 450.3698905683720000, -2.051577885510841163E-15 ) ) ;
#5361 = CARTESIAN_POINT ( 'NONE',  ( -32.02117626164387332, 50.55271151534634555, -49.49072515476203904 ) ) ;
#5362 = CARTESIAN_POINT ( 'NONE',  ( -25.35362745456398059, 262.5573905683720000, -16.75240474999999307 ) ) ;
#5363 = ORIENTED_EDGE ( 'NONE', *, *, #557, .F. ) ;
#5364 = CARTESIAN_POINT ( 'NONE',  ( -21.03221929538690205, 270.3698905601784759, 18.47759065022572500 ) ) ;
#5365 = CARTESIAN_POINT ( 'NONE',  ( -45.43829269268872650, 495.0573905683719431, -3.332260488124726638 ) ) ;
#5366 = ORIENTED_EDGE ( 'NONE', *, *, #2802, .F. ) ;
#5367 = CARTESIAN_POINT ( 'NONE',  ( -13.20868407381887089, 469.7448905683720568, 6.410867750099229490 ) ) ;
#5368 = FACE_OUTER_BOUND ( 'NONE', #18444, .T. ) ;
#5369 = CARTESIAN_POINT ( 'NONE',  ( -14.48388495494898720, 259.8073905683720000, -9.489475012073736337 ) ) ;
#5370 = EDGE_CURVE ( 'NONE', #17507, #16345, #4883, .T. ) ;
#5371 = EDGE_LOOP ( 'NONE', ( #11785, #18087, #14338, #16329, #16409, #8454, #9476, #16984, #17255, #16905, #15469, #19552, #18190, #5002, #772, #5607, #7678, #8260, #6858, #20036, #4894, #14599, #1474, #20974, #8831, #11872 ) ) ;
#5372 = CARTESIAN_POINT ( 'NONE',  ( 0.000000000000000000, -5.629165124598848990, -3.250000000000004441 ) ) ;
#5373 = EDGE_CURVE ( 'NONE', #14145, #6799, #18417, .T. ) ;
#5374 = DIRECTION ( 'NONE',  ( -1.000000000000000000, -0.000000000000000000, -0.000000000000000000 ) ) ;
#5375 = CARTESIAN_POINT ( 'NONE',  ( -35.09675569278793716, 237.2448905683720000, 15.47720386886985366 ) ) ;
#5376 = CARTESIAN_POINT ( 'NONE',  ( -45.64106924314017277, 308.1823905601784759, 11.32908994701042538 ) ) ;
#5377 = CARTESIAN_POINT ( 'NONE',  ( -42.82802356641964536, 225.9948905601784759, -14.14213562373094746 ) ) ;
#5378 = CARTESIAN_POINT ( 'NONE',  ( -28.68588794268870501, 271.3698905683720000, -16.75240474999999307 ) ) ;
#5379 = CARTESIAN_POINT ( 'NONE',  ( -13.20868407381885845, 350.9948905683720000, -6.410867750099233042 ) ) ;
#5380 = EDGE_CURVE ( 'NONE', #21185, #9090, #13228, .T. ) ;
#5381 = CARTESIAN_POINT ( 'NONE',  ( -17.35679799567827786, 280.6823905601784759, 16.95518130045146421 ) ) ;
#5382 = EDGE_CURVE ( 'NONE', #12221, #5798, #8113, .T. ) ;
#5383 = AXIS2_PLACEMENT_3D ( 'NONE', #12903, #16688, #6605 ) ;
#5384 = CARTESIAN_POINT ( 'NONE',  ( -40.53162694259544452, 402.6198905683720568, -11.84573899990672707 ) ) ;
#5385 = CARTESIAN_POINT ( 'NONE',  ( -8.685887942688738761, 512.2448905601784190, -2.449293598294705724E-15 ) ) ;
#5386 = CARTESIAN_POINT ( 'NONE',  ( -14.54375231895777532, 413.4948905601784759, -14.14213562373094746 ) ) ;
#5387 = VECTOR ( 'NONE', #948, 1000.000000000000000 ) ;
#5388 = ORIENTED_EDGE ( 'NONE', *, *, #6057, .F. ) ;
#5389 = CARTESIAN_POINT ( 'NONE',  ( -45.64106924314017988, 351.0573905765656377, -11.32908994701042538 ) ) ;
#5390 = ORIENTED_EDGE ( 'NONE', *, *, #8818, .F. ) ;
#5391 = EDGE_LOOP ( 'NONE', ( #7843, #5609 ) ) ;
#5392 = CARTESIAN_POINT ( 'NONE',  ( -28.68588794268872988, 517.8698905683720568, 16.75240474999999307 ) ) ;
#5393 = CARTESIAN_POINT ( 'NONE',  ( -24.70764059509555111, 284.4323905601784759, -19.99999999999999289 ) ) ;
#5394 = CARTESIAN_POINT ( 'NONE',  ( 0.000000000000000000, 0.000000000000000000, 0.000000000000000000 ) ) ;
#5395 =( BOUNDED_CURVE ( )  B_SPLINE_CURVE ( 3, ( #2440, #7501, #12279, #2650 ),
 .UNSPECIFIED., .F., .T. ) 
 B_SPLINE_CURVE_WITH_KNOTS ( ( 4, 4 ),
 ( 4.712388980384689674, 6.260350157286452166 ),
 .UNSPECIFIED. ) 
 CURVE ( )  GEOMETRIC_REPRESENTATION_ITEM ( )  RATIONAL_B_SPLINE_CURVE ( ( 1.000000000000000000, 0.8100893075783979214, 0.8100893075783979214, 1.000000000000000000 ) ) 
 REPRESENTATION_ITEM ( '' )  );
#5396 = EDGE_CURVE ( 'NONE', #4208, #629, #8043, .T. ) ;
#5397 = CARTESIAN_POINT ( 'NONE',  ( -38.17536295476245556, 333.8073905683720000, -14.20200298773971426 ) ) ;
#5398 = ORIENTED_EDGE ( 'NONE', *, *, #18124, .F. ) ;
#5399 = CARTESIAN_POINT ( 'NONE',  ( -14.48388495494899786, 339.8073905683720568, -9.489475012073736337 ) ) ;
#5400 = CARTESIAN_POINT ( 'NONE',  ( -32.01814843081344719, 366.0573905683720568, 16.75240474999999307 ) ) ;
#5401 = VECTOR ( 'NONE', #19415, 1000.000000000000000 ) ;
#5402 = CARTESIAN_POINT ( 'NONE',  ( -17.35679799567828496, 305.4323905765655809, 16.95518130045146421 ) ) ;
#5403 = CARTESIAN_POINT ( 'NONE',  ( -48.68588794268869435, 261.9948905765655809, 0.000000000000000000 ) ) ;
#5404 = CARTESIAN_POINT ( 'NONE',  ( -22.27502019258946575, 266.9948905683720000, 15.47720386886985189 ) ) ;
#5405 = CARTESIAN_POINT ( 'NONE',  ( -42.91927816222972325, 203.5270276421415474, 4.734255112268844101 ) ) ;
#5406 = CARTESIAN_POINT ( 'NONE',  ( -11.93348319268872793, 420.0573905683720000, 3.332260488124728415 ) ) ;
#5407 = AXIS2_PLACEMENT_3D ( 'NONE', #942, #7509, #9460 ) ;
#5408 = FACE_OUTER_BOUND ( 'NONE', #20228, .T. ) ;
#5409 = CARTESIAN_POINT ( 'NONE',  ( -47.16347859291445843, 451.3698905765656377, -7.653668647301793193 ) ) ;
#5410 = LINE ( 'NONE', #2289, #14633 ) ;
#5411 = CARTESIAN_POINT ( 'NONE',  ( -45.43829269268870519, 335.6823905683720568, 3.332260488124734632 ) ) ;
#5412 = CARTESIAN_POINT ( 'NONE',  ( -40.53162694259545162, 462.6198905683720000, -11.84573899990672707 ) ) ;
#5413 = VERTEX_POINT ( 'NONE', #3584 ) ;
#5414 = CARTESIAN_POINT ( 'NONE',  ( -17.35679799567830983, 473.8073905601784190, -16.95518130045146421 ) ) ;
#5415 = CARTESIAN_POINT ( 'NONE',  ( -45.43829269268870519, 283.8698905683720568, 0.000000000000000000 ) ) ;
#5416 = VECTOR ( 'NONE', #15430, 1000.000000000000000 ) ;
#5417 = ORIENTED_EDGE ( 'NONE', *, *, #2481, .T. ) ;
#5418 = CARTESIAN_POINT ( 'NONE',  ( -17.35679799567828496, 340.6823905601785896, 16.95518130045146421 ) ) ;
#5419 = ORIENTED_EDGE ( 'NONE', *, *, #1712, .F. ) ;
#5420 = CARTESIAN_POINT ( 'NONE',  ( -28.68588794268874054, 573.2448905601785327, 0.000000000000000000 ) ) ;
#5421 = EDGE_CURVE ( 'NONE', #7041, #3989, #8029, .T. ) ;
#5422 = CARTESIAN_POINT ( 'NONE',  ( -8.685887942688720997, 342.2448905601784759, -2.449293598294705724E-15 ) ) ;
#5423 = CARTESIAN_POINT ( 'NONE',  ( -45.43829269268869808, 293.5573905683720568, -3.332260488124726194 ) ) ;
#5424 = AXIS2_PLACEMENT_3D ( 'NONE', #9321, #15939, #11158 ) ;
#5425 = CARTESIAN_POINT ( 'NONE',  ( -28.68588794268871567, 387.8698905683720000, 16.75240474999999307 ) ) ;
#5426 = CARTESIAN_POINT ( 'NONE',  ( 71.32175588950862277, 75.31183677523708297, 94.99999999999994316 ) ) ;
#5427 = CARTESIAN_POINT ( 'NONE',  ( -17.35679799567829207, 385.4323905765655809, 16.95518130045146421 ) ) ;
#5428 = CARTESIAN_POINT ( 'NONE',  ( -14.48388495494900496, 417.9323905683720568, 9.489475012073732785 ) ) ;
#5429 = CARTESIAN_POINT ( 'NONE',  ( -11.93348319268870839, 260.3698905683720000, -2.051577885510841163E-15 ) ) ;
#5430 = CARTESIAN_POINT ( 'NONE',  ( -22.27502019258949417, 420.7448905683720000, -15.47720386886985544 ) ) ;
#5431 = CARTESIAN_POINT ( 'NONE',  ( -28.68588794268871567, 359.4948905765656377, -19.99999999999999289 ) ) ;
#5432 = CARTESIAN_POINT ( 'NONE',  ( -11.73070664223723902, 273.1823905601785327, -11.32908994701042538 ) ) ;
#5433 = CARTESIAN_POINT ( 'NONE',  ( -11.93348319268871549, 318.8698905683720000, -2.051577885510841163E-15 ) ) ;
#5434 =( NAMED_UNIT ( * ) PLANE_ANGLE_UNIT ( ) SI_UNIT ( $, .RADIAN. ) );
#5435 = CARTESIAN_POINT ( 'NONE',  ( -28.68588794268872633, 467.8698905683720000, 16.75240474999999307 ) ) ;
#5436 = CIRCLE ( 'NONE', #12002, 20.00000000000000000 ) ;
#5437 = CARTESIAN_POINT ( 'NONE',  ( -32.66413529028187668, 434.1823905765656377, 19.99999999999999289 ) ) ;
#5438 = CARTESIAN_POINT ( 'NONE',  ( -49.57497958038185715, 160.1716627696692683, -60.00000000000000000 ) ) ;
#5439 = CARTESIAN_POINT ( 'NONE',  ( -8.685887942688706786, 226.9948905765656377, -2.449293598294705724E-15 ) ) ;
#5440 = EDGE_CURVE ( 'NONE', #16962, #14726, #15171, .T. ) ;
#5441 = VECTOR ( 'NONE', #5492, 1000.000000000000000 ) ;
#5442 = CARTESIAN_POINT ( 'NONE',  ( -16.84014894278199392, 381.6198905683720568, -11.84573899990672707 ) ) ;
#5443 = DIRECTION ( 'NONE',  ( -0.000000000000000000, 1.000000000000000000, -1.224646799147353207E-16 ) ) ;
#5444 = CARTESIAN_POINT ( 'NONE',  ( -40.01497788969915348, 528.8073905601785327, 16.95518130045146776 ) ) ;
#5445 = CARTESIAN_POINT ( 'NONE',  ( -16.84014894278198682, 347.6198905683720000, 11.84573899990672530 ) ) ;
#5446 = ORIENTED_EDGE ( 'NONE', *, *, #5300, .F. ) ;
#5447 = CARTESIAN_POINT ( 'NONE',  ( -13.20868407381888154, 529.4948905683720568, -6.410867750099233042 ) ) ;
#5448 = EDGE_LOOP ( 'NONE', ( #20546, #1445, #35, #8556, #6297, #18543, #15558, #632, #17197, #21209, #8185, #12544 ) ) ;
#5449 = PRODUCT_DEFINITION ( 'UNKNOWN', '', #17987, #5099 ) ;
#5450 = CARTESIAN_POINT ( 'NONE',  ( 28.16023193154655502, 323.8848358243226357, -20.00000000000000355 ) ) ;
#5451 = CARTESIAN_POINT ( 'NONE',  ( -10.20829729246297646, 287.6198905765656377, -7.653668647301794969 ) ) ;
#5452 = DIRECTION ( 'NONE',  ( 0.000000000000000000, -1.000000000000000000, 0.000000000000000000 ) ) ;
#5453 = CARTESIAN_POINT ( 'NONE',  ( -45.43829269268871940, 493.5573905683720568, -3.332260488124726194 ) ) ;
#5454 = VERTEX_POINT ( 'NONE', #16471 ) ;
#5455 = CARTESIAN_POINT ( 'NONE',  ( -19.19641293061500065, 490.4323905683720568, -14.20200298773971603 ) ) ;
#5456 = CARTESIAN_POINT ( 'NONE',  ( -13.63080313027055901, 49.23037255044063443, -47.26215086388379660 ) ) ;
#5457 = EDGE_CURVE ( 'NONE', #11304, #1316, #19019, .T. ) ;
#5458 = CARTESIAN_POINT ( 'NONE',  ( -11.73070664223725323, 416.0573905765656377, 11.32908994701042005 ) ) ;
#5459 = DIRECTION ( 'NONE',  ( 0.000000000000000000, -1.000000000000000000, 0.000000000000000000 ) ) ;
#5460 = CARTESIAN_POINT ( 'NONE',  ( 1.631480618821192334E-14, 213.9102039777116602, -24.99999999999999645 ) ) ;
#5461 = CARTESIAN_POINT ( 'NONE',  ( -48.68588794268872277, 487.2448905601784759, 0.000000000000000000 ) ) ;
#5462 = CARTESIAN_POINT ( 'NONE',  ( 35.96497763894178945, 230.5765313837437418, 60.00000000000000000 ) ) ;
#5463 =( BOUNDED_CURVE ( )  B_SPLINE_CURVE ( 2, ( #13891, #12258, #18841, #2421, #10621, #20583, #12685, #916, #4251, #4134, #14004, #2525, #9108, #1227, #19069, #15730, #2632 ),
 .UNSPECIFIED., .F., .T. ) 
 B_SPLINE_CURVE_WITH_KNOTS ( ( 3, 2, 2, 2, 2, 2, 2, 2, 3 ),
 ( 0.04687500000000040246, 0.04882812500000036082, 0.05078125000000031919, 0.05273437500000027062, 0.05468750000000022898, 0.05664062500000018735, 0.05859375000000013878, 0.06054687500000009714, 0.06250000000000005551 ),
 .UNSPECIFIED. ) 
 CURVE ( )  GEOMETRIC_REPRESENTATION_ITEM ( )  RATIONAL_B_SPLINE_CURVE ( ( 0.9999999999999960032, 0.9807852804032344274, 1.000000000000000000, 0.9807852804032304306, 1.000000000000000000, 0.9807852804032304306, 1.000000000000000000, 0.9807852804032304306, 1.000000000000000000, 0.9807852804032304306, 1.000000000000000000, 0.9807852804032304306, 1.000000000000000000, 0.9807852804032304306, 1.000000000000000000, 0.9807852804032298755, 1.000000000000000444 ) ) 
 REPRESENTATION_ITEM ( '' )  );
#5464 = LINE ( 'NONE', #1731, #10962 ) ;
#5465 = CARTESIAN_POINT ( 'NONE',  ( -17.35679799567827786, 240.6823905601784759, 16.95518130045146421 ) ) ;
#5466 = CARTESIAN_POINT ( 'NONE',  ( 0.2578475836320708869, -4.367703157927327773, 5.434916218090835471 ) ) ;
#5467 = CARTESIAN_POINT ( 'NONE',  ( -11.93348319268871371, 290.0573905683720000, 3.332260488124728415 ) ) ;
#5468 = EDGE_CURVE ( 'NONE', #349, #7167, #16222, .T. ) ;
#5469 = CARTESIAN_POINT ( 'NONE',  ( -14.54375231895775400, 233.4948905601784759, -14.14213562373094746 ) ) ;
#5470 = ADVANCED_FACE ( 'NONE', ( #8654 ), #10486, .F. ) ;
#5471 = CARTESIAN_POINT ( 'NONE',  ( -22.27502019258949773, 442.2448905683720000, -15.47720386886985544 ) ) ;
#5472 = DIRECTION ( 'NONE',  ( -1.000000000000000000, 0.000000000000000000, 0.000000000000000000 ) ) ;
#5473 = CARTESIAN_POINT ( 'NONE',  ( -22.27502019258947641, 272.2448905683720568, -15.47720386886985544 ) ) ;
#5474 = ORIENTED_EDGE ( 'NONE', *, *, #6268, .T. ) ;
#5475 = CARTESIAN_POINT ( 'NONE',  ( -10.20829729246300666, 532.8698905601785327, -7.653668647301794969 ) ) ;
#5476 = CARTESIAN_POINT ( 'NONE',  ( -11.93348319268873503, 480.0573905683720568, 3.332260488124728859 ) ) ;
#5477 = ORIENTED_EDGE ( 'NONE', *, *, #16647, .T. ) ;
#5478 = CARTESIAN_POINT ( 'NONE',  ( -42.88789093042844058, 426.3073905683720000, 9.489475012073734561 ) ) ;
#5479 = CYLINDRICAL_SURFACE ( 'NONE', #9684, 6.500000000000000888 ) ;
#5480 = CARTESIAN_POINT ( 'NONE',  ( -25.35362745456397704, 251.0573905683720000, -16.75240474999999307 ) ) ;
#5481 = ORIENTED_EDGE ( 'NONE', *, *, #10278, .T. ) ;
#5482 = DIRECTION ( 'NONE',  ( 0.8865057725575725689, 0.000000000000000000, 0.4627175328665443232 ) ) ;
#5483 = VECTOR ( 'NONE', #7179, 1000.000000000000114 ) ;
#5484 = CARTESIAN_POINT ( 'NONE',  ( -35.09675569278793716, 273.4948905683720000, -15.47720386886985544 ) ) ;
#5485 = CARTESIAN_POINT ( 'NONE',  ( -28.68588794268873343, 489.4948905765656377, -19.99999999999999289 ) ) ;
#5486 = FACE_OUTER_BOUND ( 'NONE', #5954, .T. ) ;
#5487 = CARTESIAN_POINT ( 'NONE',  ( -22.27502019258946220, 248.4948905683720284, 15.47720386886985189 ) ) ;
#5488 = CARTESIAN_POINT ( 'NONE',  ( -35.09675569278797269, 507.2448905683719431, 15.47720386886985366 ) ) ;
#5489 = CARTESIAN_POINT ( 'NONE',  ( -8.685887942688706786, 232.2448905601785043, -2.449293598294705724E-15 ) ) ;
#5490 = CARTESIAN_POINT ( 'NONE',  ( -11.93348319268870661, 248.8698905683720000, -2.051577885510841163E-15 ) ) ;
#5491 = CARTESIAN_POINT ( 'NONE',  ( -22.27502019258947641, 358.4948905683720000, 15.47720386886985189 ) ) ;
#5492 = DIRECTION ( 'NONE',  ( -1.000000000000000000, 0.000000000000000000, 0.000000000000000000 ) ) ;
#5493 = AXIS2_PLACEMENT_3D ( 'NONE', #12996, #8220, #14848 ) ;
#5494 = CARTESIAN_POINT ( 'NONE',  ( -40.53162694259544452, 405.1198905683720000, 11.84573899990672885 ) ) ;
#5495 = CARTESIAN_POINT ( 'NONE',  ( -24.70764059509556532, 510.0573905601785327, 19.99999999999998934 ) ) ;
#5496 = CARTESIAN_POINT ( 'NONE',  ( -47.16347859291445133, 416.6198905601785327, -7.653668647301793193 ) ) ;
#5497 = VERTEX_POINT ( 'NONE', #15599 ) ;
#5498 = CARTESIAN_POINT ( 'NONE',  ( -8.685887942688720997, 346.9948905765656377, -2.449293598294705724E-15 ) ) ;
#5499 = ORIENTED_EDGE ( 'NONE', *, *, #21202, .T. ) ;
#5500 = ORIENTED_EDGE ( 'NONE', *, *, #6160, .T. ) ;
#5501 = CARTESIAN_POINT ( 'NONE',  ( -13.20868407381887977, 529.7448905683720568, 6.410867750099229490 ) ) ;
#5502 = CARTESIAN_POINT ( 'NONE',  ( -11.73070664223724080, 293.1823905601784759, -11.32908994701042715 ) ) ;
#5503 = CARTESIAN_POINT ( 'NONE',  ( 170.2047888904039610, 620.7448905601785327, -1.893624729818132124 ) ) ;
#5504 = VERTEX_POINT ( 'NONE', #15385 ) ;
#5505 = EDGE_CURVE ( 'NONE', #19049, #17928, #15404, .T. ) ;
#5506 = CARTESIAN_POINT ( 'NONE',  ( -22.27502019258947286, 328.4948905683720568, 15.47720386886985189 ) ) ;
#5507 = ORIENTED_EDGE ( 'NONE', *, *, #20586, .F. ) ;
#5508 = CARTESIAN_POINT ( 'NONE',  ( -13.20868407381885845, 349.4948905683720000, -6.410867750099233042 ) ) ;
#5509 = EDGE_CURVE ( 'NONE', #4217, #17801, #1408, .T. ) ;
#5510 = CARTESIAN_POINT ( 'NONE',  ( -42.88789093042843348, 374.8073905683720568, 9.489475012073734561 ) ) ;
#5511 = VECTOR ( 'NONE', #3659, 1000.000000000000000 ) ;
#5512 = EDGE_CURVE ( 'NONE', #19311, #13531, #10251, .T. ) ;
#5513 = CARTESIAN_POINT ( 'NONE',  ( -36.33955658999050087, 290.1198905765656377, -18.47759065022572855 ) ) ;
#5514 = PLANE ( 'NONE',  #18980 ) ;
#5515 = CARTESIAN_POINT ( 'NONE',  ( -14.48388495494898720, 259.8073905683720568, -9.489475012073734561 ) ) ;
#5516 = DIRECTION ( 'NONE',  ( 0.000000000000000000, 1.000000000000000000, 0.000000000000000000 ) ) ;
#5517 = CARTESIAN_POINT ( 'NONE',  ( -25.35362745456398770, 408.1823905683720568, 16.75240474999998952 ) ) ;
#5518 = CARTESIAN_POINT ( 'NONE',  ( -13.68588794268874054, 573.2448905601785327, 1.836970198721029589E-15 ) ) ;
#5519 = DIRECTION ( 'NONE',  ( -0.000000000000000000, -0.000000000000000000, -1.000000000000000000 ) ) ;
#5520 = PLANE ( 'NONE',  #19783 ) ;
#5521 = EDGE_CURVE ( 'NONE', #15324, #10233, #392, .T. ) ;
#5522 = CARTESIAN_POINT ( 'NONE',  ( -19.19641293061498288, 331.9323905683720000, -14.20200298773971603 ) ) ;
#5523 = CARTESIAN_POINT ( 'NONE',  ( -25.35362745456400546, 471.0573905683720568, -16.75240474999999307 ) ) ;
#5524 = ORIENTED_EDGE ( 'NONE', *, *, #173, .F. ) ;
#5525 = CARTESIAN_POINT ( 'NONE',  ( -21.03221929538693402, 464.1198905601784759, -18.47759065022572855 ) ) ;
#5526 = CARTESIAN_POINT ( 'NONE',  ( -32.01814843081344009, 291.6823905683720568, -16.75240474999999307 ) ) ;
#5527 = ORIENTED_EDGE ( 'NONE', *, *, #3620, .F. ) ;
#5528 = ORIENTED_EDGE ( 'NONE', *, *, #11209, .T. ) ;
#5529 = DIRECTION ( 'NONE',  ( -0.4627175328665442677, 0.000000000000000000, -0.8865057725575725689 ) ) ;
#5530 = CARTESIAN_POINT ( 'NONE',  ( -48.68588794268870856, 346.9323905601784759, -3.978247347593158345 ) ) ;
#5531 = CARTESIAN_POINT ( 'NONE',  ( -28.68588794268870501, 306.3698905683720568, 16.75240474999999307 ) ) ;
#5532 = CARTESIAN_POINT ( 'NONE',  ( -11.93348319268872437, 390.6823905683720568, -3.332260488124732856 ) ) ;
#5533 = VECTOR ( 'NONE', #10449, 1000.000000000000114 ) ;
#5534 = CARTESIAN_POINT ( 'NONE',  ( -28.68588794268871567, 374.7448905601785327, -19.99999999999999289 ) ) ;
#5535 = CARTESIAN_POINT ( 'NONE',  ( -21.03221929538693047, 525.1198905765655809, 18.47759065022572500 ) ) ;
#5536 = CARTESIAN_POINT ( 'NONE',  ( -25.35362745456399480, 401.0573905683720000, -16.75240474999999307 ) ) ;
#5537 = CARTESIAN_POINT ( 'NONE',  ( -42.88789093042841927, 254.4323905683720284, -9.489475012073736337 ) ) ;
#5538 = CARTESIAN_POINT ( 'NONE',  ( -40.53162694259544452, 432.6198905683720000, -11.84573899990672707 ) ) ;
#5539 = CARTESIAN_POINT ( 'NONE',  ( -45.64106924314018698, 352.9323905765656377, 11.32908994701042715 ) ) ;
#5540 = LINE ( 'NONE', #588, #10324 ) ;
#5541 = CARTESIAN_POINT ( 'NONE',  ( -45.43829269268871229, 333.5573905683720568, -3.332260488124726638 ) ) ;
#5542 = CARTESIAN_POINT ( 'NONE',  ( -35.09675569278796559, 477.2448905683720568, 15.47720386886985366 ) ) ;
#5543 = CARTESIAN_POINT ( 'NONE',  ( -31.26501780185373391, 205.1437886375728965, 5.000000000000001776 ) ) ;
#5544 = CARTESIAN_POINT ( 'NONE',  ( 19.47671684378140355, 160.1716627696692683, -61.31874706328063240 ) ) ;
#5545 = DIRECTION ( 'NONE',  ( -1.000000000000000000, 0.000000000000000000, 0.000000000000000000 ) ) ;
#5546 = AXIS2_PLACEMENT_3D ( 'NONE', #18305, #18093, #10185 ) ;
#5547 = CARTESIAN_POINT ( 'NONE',  ( -16.84014894278199037, 379.1198905683720568, 11.84573899990672530 ) ) ;
#5548 = AXIS2_PLACEMENT_3D ( 'NONE', #4647, #4228, #2606 ) ;
#5549 = CARTESIAN_POINT ( 'NONE',  ( -33.46524870589303902, 53.80964298180775529, -120.4371303356476091 ) ) ;
#5550 = CARTESIAN_POINT ( 'NONE',  ( -45.64106924314020119, 518.1823905601785327, 11.32908994701042715 ) ) ;
#5551 = CARTESIAN_POINT ( 'NONE',  ( -44.16309181155857289, 353.2448905683720000, -6.410867750099231266 ) ) ;
#5552 = VERTEX_POINT ( 'NONE', #17424 ) ;
#5553 = CARTESIAN_POINT ( 'NONE',  ( -14.48388495494901740, 509.8073905683720000, -9.489475012073736337 ) ) ;
#5554 = ORIENTED_EDGE ( 'NONE', *, *, #6229, .T. ) ;
#5555 = CARTESIAN_POINT ( 'NONE',  ( -17.35679799567829207, 350.6823905601785327, 16.95518130045146421 ) ) ;
#5556 = CARTESIAN_POINT ( 'NONE',  ( -8.685887942688641061, 417.3073905765655809, -3.978247347592952732 ) ) ;
#5557 = CARTESIAN_POINT ( 'NONE',  ( -14.54375231895775400, 228.2448905765656093, -14.14213562373094746 ) ) ;
#5558 = CARTESIAN_POINT ( 'NONE',  ( -28.68588794268870146, 287.8698905683720568, 16.75240474999999307 ) ) ;
#5559 = DIRECTION ( 'NONE',  ( 0.000000000000000000, -1.000000000000000000, 0.000000000000000000 ) ) ;
#5560 = PRESENTATION_STYLE_ASSIGNMENT (( #4370 ) ) ;
#5561 = CARTESIAN_POINT ( 'NONE',  ( -11.93348319268873325, 459.1823905683720000, -3.332260488124732856 ) ) ;
#5562 = VERTEX_POINT ( 'NONE', #20986 ) ;
#5563 = CARTESIAN_POINT ( 'NONE',  ( -38.17536295476246266, 485.4323905683720000, 14.20200298773971781 ) ) ;
#5564 = CARTESIAN_POINT ( 'NONE',  ( 6.416697501590670427, 172.9933428177121471, 45.00000000000000000 ) ) ;
#5565 = EDGE_CURVE ( 'NONE', #14938, #13766, #12461, .T. ) ;
#5566 = VECTOR ( 'NONE', #9797, 1000.000000000000000 ) ;
#5567 = CARTESIAN_POINT ( 'NONE',  ( -21.03221929538691626, 425.1198905765656377, 18.47759065022572500 ) ) ;
#5568 = DIRECTION ( 'NONE',  ( -0.3090169943749470072, 0.000000000000000000, 0.9510565162951536422 ) ) ;
#5569 = CARTESIAN_POINT ( 'NONE',  ( -21.03221929538690205, 300.3698905601784759, 18.47759065022572500 ) ) ;
#5570 = DIRECTION ( 'NONE',  ( 1.191790137725560488E-16, -1.000000000000000000, 0.000000000000000000 ) ) ;
#5571 = DIRECTION ( 'NONE',  ( 0.000000000000000000, 1.000000000000000000, 0.000000000000000000 ) ) ;
#5572 = CARTESIAN_POINT ( 'NONE',  ( -48.68588794268852382, 261.6823905765655809, -3.978247347593583783 ) ) ;
#5573 = PRESENTATION_STYLE_ASSIGNMENT (( #13702 ) ) ;
#5574 = ADVANCED_FACE ( 'NONE', ( #19157 ), #4331, .F. ) ;
#5575 = CARTESIAN_POINT ( 'NONE',  ( -49.57497958038186425, 230.5765313837437418, 60.00000000000000000 ) ) ;
#5576 = CARTESIAN_POINT ( 'NONE',  ( -38.17536295476244135, 286.9323905683720000, 14.20200298773971781 ) ) ;
#5577 = CARTESIAN_POINT ( 'NONE',  ( -14.54375231895775755, 253.4948905601784759, -14.14213562373094746 ) ) ;
#5578 = CARTESIAN_POINT ( 'NONE',  ( -10.20829729246299067, 406.3698905765656377, 7.653668647301790529 ) ) ;
#5579 = CARTESIAN_POINT ( 'NONE',  ( -42.88789093042844058, 446.3073905683720000, 9.489475012073736337 ) ) ;
#5580 = CARTESIAN_POINT ( 'NONE',  ( -48.68588794268858067, 401.6823905765655809, -3.978247347593477201 ) ) ;
#5581 = CARTESIAN_POINT ( 'NONE',  ( -16.84014894278197616, 269.1198905683720568, 11.84573899990672530 ) ) ;
#5582 = ORIENTED_EDGE ( 'NONE', *, *, #17769, .T. ) ;
#5583 = CARTESIAN_POINT ( 'NONE',  ( -8.685887942688742314, 573.2448905601785327, 2.449293598294706119E-15 ) ) ;
#5584 = VECTOR ( 'NONE', #21183, 1000.000000000000000 ) ;
#5585 = CARTESIAN_POINT ( 'NONE',  ( -16.84014894278200458, 491.6198905683720000, -11.84573899990672707 ) ) ;
#5586 = ORIENTED_EDGE ( 'NONE', *, *, #11731, .F. ) ;
#5587 = CARTESIAN_POINT ( 'NONE',  ( -21.03221929538693047, 525.1198905765655809, 18.47759065022572500 ) ) ;
#5588 = CARTESIAN_POINT ( 'NONE',  ( -42.88789093042841927, 252.9323905683720284, -9.489475012073736337 ) ) ;
#5589 = ORIENTED_EDGE ( 'NONE', *, *, #9958, .T. ) ;
#5590 =( BOUNDED_CURVE ( )  B_SPLINE_CURVE ( 2, ( #10089, #6627, #11503, #18100, #9981, #5013, #16390, #9765, #19616, #4793, #13248, #1565, #18313, #15091, #8358, #3503, #14766 ),
 .UNSPECIFIED., .F., .T. ) 
 B_SPLINE_CURVE_WITH_KNOTS ( ( 3, 2, 2, 2, 2, 2, 2, 2, 3 ),
 ( 0.8437500000000002220, 0.8457031250000002220, 0.8476562500000002220, 0.8496093750000002220, 0.8515625000000002220, 0.8535156250000002220, 0.8554687500000002220, 0.8574218750000002220, 0.8593750000000002220 ),
 .UNSPECIFIED. ) 
 CURVE ( )  GEOMETRIC_REPRESENTATION_ITEM ( )  RATIONAL_B_SPLINE_CURVE ( ( 0.9999999999999977796, 0.9807852804032326510, 1.000000000000000000, 0.9807852804032304306, 1.000000000000000000, 0.9807852804032304306, 1.000000000000000000, 0.9807852804032304306, 1.000000000000000000, 0.9807852804032304306, 1.000000000000000000, 0.9807852804032304306, 1.000000000000000000, 0.9807852804032304306, 1.000000000000000000, 0.9807852804032282101, 1.000000000000002220 ) ) 
 REPRESENTATION_ITEM ( '' )  );
#5591 = CARTESIAN_POINT ( 'NONE',  ( -28.68588794268869790, 213.9102039777116602, 0.000000000000000000 ) ) ;
#5592 = EDGE_CURVE ( 'NONE', #11897, #18587, #12874, .T. ) ;
#5593 = CARTESIAN_POINT ( 'NONE',  ( -40.01497788969915348, 480.4323905765655809, -16.95518130045146421 ) ) ;
#5594 = CARTESIAN_POINT ( 'NONE',  ( 0.5805565836007611225, 3.752776749732563033, 6.500000000000000000 ) ) ;
#5595 = FACE_OUTER_BOUND ( 'NONE', #11007, .T. ) ;
#5596 = CARTESIAN_POINT ( 'NONE',  ( -14.48388495494898365, 249.4323905683720284, 9.489475012073731008 ) ) ;
#5597 = CARTESIAN_POINT ( 'NONE',  ( -35.09675569278797269, 517.2448905683719431, 15.47720386886985366 ) ) ;
#5598 = CARTESIAN_POINT ( 'NONE',  ( -8.938426032941704028E-16, 600.7448905601785327, -7.500000000000000000 ) ) ;
#5599 = CARTESIAN_POINT ( 'NONE',  ( -14.48388495494898542, 249.8073905683720568, -9.489475012073736337 ) ) ;
#5600 = CARTESIAN_POINT ( 'NONE',  ( -13.20868407381885667, 330.9948905683720000, -6.410867750099233042 ) ) ;
#5601 = CARTESIAN_POINT ( 'NONE',  ( -10.20829729246298001, 321.6198905601784759, 7.653668647301790529 ) ) ;
#5602 = ADVANCED_FACE ( 'NONE', ( #6052 ), #9188, .F. ) ;
#5603 = CARTESIAN_POINT ( 'NONE',  ( -13.20868407381886378, 408.2448905683720568, 6.410867750099229490 ) ) ;
#5604 = CARTESIAN_POINT ( 'NONE',  ( -8.685887942688719221, 326.9948905765656377, -2.449293598294705724E-15 ) ) ;
#5605 = AXIS2_PLACEMENT_3D ( 'NONE', #20957, #13054, #16313 ) ;
#5606 = CARTESIAN_POINT ( 'NONE',  ( -17.35679799567830273, 403.8073905601785327, -16.95518130045146421 ) ) ;
#5607 = ORIENTED_EDGE ( 'NONE', *, *, #9290, .T. ) ;
#5608 = CARTESIAN_POINT ( 'NONE',  ( 0.000000000000000000, 4.898587196589412829E-16, -4.000000000000000000 ) ) ;
#5609 = ORIENTED_EDGE ( 'NONE', *, *, #7649, .F. ) ;
#5610 = EDGE_LOOP ( 'NONE', ( #13683, #14889, #1365, #9706, #12452, #12724 ) ) ;
#5611 = CARTESIAN_POINT ( 'NONE',  ( -44.16309181155859420, 514.7448905683720568, -6.410867750099231266 ) ) ;
#5612 = CARTESIAN_POINT ( 'NONE',  ( -40.01497788969913216, 320.4323905765656377, -16.95518130045146421 ) ) ;
#5613 = VERTEX_POINT ( 'NONE', #6262 ) ;
#5614 = ADVANCED_FACE ( 'NONE', ( #20665 ), #12767, .F. ) ;
#5615 = CARTESIAN_POINT ( 'NONE',  ( -42.88789093042842637, 324.4323905683720000, -9.489475012073734561 ) ) ;
#5616 = ORIENTED_EDGE ( 'NONE', *, *, #5775, .F. ) ;
#5617 = CARTESIAN_POINT ( 'NONE',  ( -16.84014894278198682, 347.6198905683720000, 11.84573899990672530 ) ) ;
#5618 = CARTESIAN_POINT ( 'NONE',  ( -44.16309181155856578, 354.4948905683720000, 6.410867750099241924 ) ) ;
#5619 = CARTESIAN_POINT ( 'NONE',  ( -45.64106924314017988, 291.0573905765656377, -11.32908994701042715 ) ) ;
#5620 = CARTESIAN_POINT ( 'NONE',  ( -36.33955658999052218, 500.1198905765655809, -18.47759065022572855 ) ) ;
#5621 = CARTESIAN_POINT ( 'NONE',  ( -13.20868407381884602, 248.2448905683720000, 6.410867750099229490 ) ) ;
#5622 = CARTESIAN_POINT ( 'NONE',  ( -43.58160426315849634, 200.4655464737082582, 1.772246553899823329 ) ) ;
#5623 = CARTESIAN_POINT ( 'NONE',  ( -14.48388495494900496, 411.3073905683720000, -9.489475012073736337 ) ) ;
#5624 = DIRECTION ( 'NONE',  ( -1.191790137725560488E-16, 1.000000000000000000, -0.000000000000000000 ) ) ;
#5625 = CARTESIAN_POINT ( 'NONE',  ( -28.68588794268869435, 193.9102039777116602, 0.000000000000000000 ) ) ;
#5626 = CARTESIAN_POINT ( 'NONE',  ( 0.000000000000000000, 610.7448905601785327, 0.000000000000000000 ) ) ;
#5627 = CARTESIAN_POINT ( 'NONE',  ( -13.20868407381885135, 309.7448905683720568, 6.410867750099229490 ) ) ;
#5628 = CARTESIAN_POINT ( 'NONE',  ( -14.48388495494900852, 457.9323905683720568, 9.489475012073732785 ) ) ;
#5629 = ORIENTED_EDGE ( 'NONE', *, *, #2095, .F. ) ;
#5630 = CARTESIAN_POINT ( 'NONE',  ( -24.70764059509557242, 464.4323905601784759, -19.99999999999999289 ) ) ;
#5631 = CARTESIAN_POINT ( 'NONE',  ( -42.88789093042842637, 292.9323905683720568, -9.489475012073736337 ) ) ;
#5632 = VECTOR ( 'NONE', #14090, 1000.000000000000000 ) ;
#5633 = ORIENTED_EDGE ( 'NONE', *, *, #20396, .T. ) ;
#5634 = LINE ( 'NONE', #17220, #3226 ) ;
#5635 = CARTESIAN_POINT ( 'NONE',  ( -14.48388495494900674, 439.4323905683719431, 9.489475012073731008 ) ) ;
#5636 = ORIENTED_EDGE ( 'NONE', *, *, #6246, .T. ) ;
#5637 = DIRECTION ( 'NONE',  ( -1.000000000000000000, 0.000000000000000000, -0.000000000000000000 ) ) ;
#5638 = AXIS2_PLACEMENT_3D ( 'NONE', #2872, #4488, #9025 ) ;
#5639 = CARTESIAN_POINT ( 'NONE',  ( -13.20868407381885490, 309.4948905683720568, -6.410867750099233042 ) ) ;
#5640 = CARTESIAN_POINT ( 'NONE',  ( -32.01814843081344719, 377.5573905683721136, 16.75240474999999307 ) ) ;
#5641 = CARTESIAN_POINT ( 'NONE',  ( -36.33955658999050087, 229.1198905601785043, 18.47759065022572500 ) ) ;
#5642 = CARTESIAN_POINT ( 'NONE',  ( -8.685887942688744090, 527.3073905765656946, -3.978247347593165895 ) ) ;
#5643 = CARTESIAN_POINT ( 'NONE',  ( -35.09675569278795848, 395.7448905683720568, 15.47720386886985366 ) ) ;
#5644 = CARTESIAN_POINT ( 'NONE',  ( -32.01814843081343298, 247.5573905683720000, 16.75240474999999307 ) ) ;
#5645 = ADVANCED_FACE ( 'NONE', ( #15814 ), #14082, .T. ) ;
#5646 = CARTESIAN_POINT ( 'NONE',  ( -19.19641293061498999, 430.4323905683720000, -14.20200298773971603 ) ) ;
#5647 = EDGE_CURVE ( 'NONE', #2506, #14726, #2928, .T. ) ;
#5648 = CARTESIAN_POINT ( 'NONE',  ( -40.01497788969913216, 353.5573905765656377, 16.95518130045146776 ) ) ;
#5649 = CARTESIAN_POINT ( 'NONE',  ( 29.72350413846044859, 280.4463447002762564, 40.00000000000000000 ) ) ;
#5650 = CARTESIAN_POINT ( 'NONE',  ( -38.17536295476244845, 302.3073905683720568, -14.20200298773971426 ) ) ;
#5651 = CARTESIAN_POINT ( 'NONE',  ( -35.09675569278795848, 483.4948905683720000, -15.47720386886985544 ) ) ;
#5652 = VECTOR ( 'NONE', #16060, 1000.000000000000000 ) ;
#5653 = CARTESIAN_POINT ( 'NONE',  ( -8.685887942688715668, 302.2448905601784190, -2.449293598294705724E-15 ) ) ;
#5654 = FACE_OUTER_BOUND ( 'NONE', #17798, .T. ) ;
#5655 = DIRECTION ( 'NONE',  ( 0.4989387216749511800, 0.8666372666885294729, 0.000000000000000000 ) ) ;
#5656 = AXIS2_PLACEMENT_3D ( 'NONE', #11316, #12845, #4619 ) ;
#5657 = CARTESIAN_POINT ( 'NONE',  ( -32.01814843081344719, 377.5573905683720568, 16.75240474999999307 ) ) ;
#5658 = CARTESIAN_POINT ( 'NONE',  ( -29.89242224052212293, 48.12632300629133653, -121.3744031878869976 ) ) ;
#5659 = CARTESIAN_POINT ( 'NONE',  ( -32.66413529028189799, 535.0573905601784190, -19.99999999999999289 ) ) ;
#5660 = CARTESIAN_POINT ( 'NONE',  ( -19.19641293061498288, 340.4323905683720000, -14.20200298773971603 ) ) ;
#5661 = ORIENTED_EDGE ( 'NONE', *, *, #13857, .F. ) ;
#5662 = CARTESIAN_POINT ( 'NONE',  ( -45.43829269268871940, 504.1823905683721136, 3.332260488124734632 ) ) ;
#5663 = VERTEX_POINT ( 'NONE', #16124 ) ;
#5664 = CARTESIAN_POINT ( 'NONE',  ( 78.68120802659204571, 149.7457237375499517, 20.00000000000000355 ) ) ;
#5665 = CARTESIAN_POINT ( 'NONE',  ( -48.68588794268887199, 312.3073905765655240, 3.978247347592742678 ) ) ;
#5666 = CARTESIAN_POINT ( 'NONE',  ( -48.68588794268870146, 291.9948905765656377, 0.000000000000000000 ) ) ;
#5667 = CARTESIAN_POINT ( 'NONE',  ( 4.700000000000000178, -5.629165124598848990, -3.250000000000005329 ) ) ;
#5668 = CARTESIAN_POINT ( 'NONE',  ( -14.48388495494901029, 459.8073905683720000, -9.489475012073736337 ) ) ;
#5669 = VERTEX_POINT ( 'NONE', #7563 ) ;
#5670 = CARTESIAN_POINT ( 'NONE',  ( -38.17536295476246977, 482.3073905683720000, -14.20200298773971426 ) ) ;
#5671 = CARTESIAN_POINT ( 'NONE',  ( -40.01497788969911795, 248.8073905601784759, 16.95518130045146776 ) ) ;
#5672 = AXIS2_PLACEMENT_3D ( 'NONE', #1112, #18936, #5637 ) ;
#5673 = CARTESIAN_POINT ( 'NONE',  ( -48.68588794268871567, 411.6823905765656377, -3.978247347593158345 ) ) ;
#5674 = CARTESIAN_POINT ( 'NONE',  ( -18.81370552131602736, 600.7448905601785327, -6.112943483001347822 ) ) ;
#5675 = DIRECTION ( 'NONE',  ( 1.000000000000000000, 1.191790137725560488E-16, 1.178908271762451515E-16 ) ) ;
#5676 = CARTESIAN_POINT ( 'NONE',  ( -10.20829729246299955, 482.8698905601784759, -7.653668647301794969 ) ) ;
#5677 = CARTESIAN_POINT ( 'NONE',  ( -41.83569717483972994, 213.9102039777116602, -25.00000000000000000 ) ) ;
#5678 = CARTESIAN_POINT ( 'NONE',  ( 81.24038404635966515, 10.52886280891152104, -94.99999999999994316 ) ) ;
#5679 = CARTESIAN_POINT ( 'NONE',  ( -36.33955658999050087, 239.1198905601784475, 18.47759065022572500 ) ) ;
#5680 = PLANE ( 'NONE',  #15592 ) ;
#5681 = CARTESIAN_POINT ( 'NONE',  ( -44.16309181155855867, 285.9948905683720000, 6.410867750099241924 ) ) ;
#5682 = CARTESIAN_POINT ( 'NONE',  ( -10.20829729246297291, 251.6198905601784759, 7.653668647301790529 ) ) ;
#5683 = CARTESIAN_POINT ( 'NONE',  ( -17.35679799567829562, 405.4323905765655240, 16.95518130045146421 ) ) ;
#5684 = CARTESIAN_POINT ( 'NONE',  ( -19.19641293061499354, 441.9323905683720568, -14.20200298773971603 ) ) ;
#5685 = CARTESIAN_POINT ( 'NONE',  ( -36.33955658999051508, 400.1198905765656377, -18.47759065022572855 ) ) ;
#5686 = CARTESIAN_POINT ( 'NONE',  ( -11.93348319268871016, 260.6823905683720000, -3.332260488124732856 ) ) ;
#5687 = ORIENTED_EDGE ( 'NONE', *, *, #20422, .F. ) ;
#5688 = ORIENTED_EDGE ( 'NONE', *, *, #14401, .T. ) ;
#5689 = CARTESIAN_POINT ( 'NONE',  ( -25.35362745456399480, 488.1823905683720568, 16.75240474999998952 ) ) ;
#5690 = ORIENTED_EDGE ( 'NONE', *, *, #9426, .F. ) ;
#5691 = DIRECTION ( 'NONE',  ( -1.191790137725560488E-16, 1.000000000000000000, -0.000000000000000000 ) ) ;
#5692 = CARTESIAN_POINT ( 'NONE',  ( -42.88789093042841927, 232.9323905683720000, -9.489475012073736337 ) ) ;
#5693 = ORIENTED_EDGE ( 'NONE', *, *, #20663, .T. ) ;
#5694 = CYLINDRICAL_SURFACE ( 'NONE', #13513, 15.00000000000000000 ) ;
#5695 = CARTESIAN_POINT ( 'NONE',  ( -32.66413529028189089, 454.1823905765656377, 19.99999999999999289 ) ) ;
#5696 = CARTESIAN_POINT ( 'NONE',  ( -21.03221929538691626, 308.8698905765655809, -18.47759065022572855 ) ) ;
#5697 = CARTESIAN_POINT ( 'NONE',  ( -38.22409075892743857, 223.9102039777116886, -13.96110877218534085 ) ) ;
#5698 = DIRECTION ( 'NONE',  ( 1.000000000000000000, 1.250996701150283068E-16, -0.000000000000000000 ) ) ;
#5699 = VECTOR ( 'NONE', #18581, 1000.000000000000000 ) ;
#5700 = CARTESIAN_POINT ( 'NONE',  ( -35.09675569278796559, 513.4948905683720568, -15.47720386886985544 ) ) ;
#5701 = DIRECTION ( 'NONE',  ( 1.000000000000000000, 0.000000000000000000, 0.000000000000000000 ) ) ;
#5702 = CARTESIAN_POINT ( 'NONE',  ( -28.68588794268870146, 251.3698905683720000, -16.75240474999999307 ) ) ;
#5703 = CARTESIAN_POINT ( 'NONE',  ( -44.16309181155857289, 344.7448905683720568, -6.410867750099231266 ) ) ;
#5704 = CARTESIAN_POINT ( 'NONE',  ( -45.64106924314019409, 468.1823905601785327, 11.32908994701042538 ) ) ;
#5705 = ADVANCED_FACE ( 'NONE', ( #10914 ), #17526, .T. ) ;
#5706 = CARTESIAN_POINT ( 'NONE',  ( -14.48388495494900141, 379.8073905683720568, -9.489475012073736337 ) ) ;
#5707 = CARTESIAN_POINT ( 'NONE',  ( -24.70764059509554755, 324.8073905765656377, 19.99999999999998934 ) ) ;
#5708 =( BOUNDED_CURVE ( )  B_SPLINE_CURVE ( 2, ( #7416, #15985, #14042, #20624, #2673, #1166, #5587, #7739, #5799, #4182, #16303, #4708, #17901, #9783, #16085, #19743, #9679 ),
 .UNSPECIFIED., .F., .T. ) 
 B_SPLINE_CURVE_WITH_KNOTS ( ( 3, 2, 2, 2, 2, 2, 2, 2, 3 ),
 ( 0.01562500000000037470, 0.01757812500000033307, 0.01953125000000028796, 0.02148437500000024286, 0.02343750000000020123, 0.02539062500000015959, 0.02734375000000011449, 0.02929687500000006939, 0.03125000000000002776 ),
 .UNSPECIFIED. ) 
 CURVE ( )  GEOMETRIC_REPRESENTATION_ITEM ( )  RATIONAL_B_SPLINE_CURVE ( ( 0.9999999999999963363, 0.9807852804032340943, 1.000000000000000000, 0.9807852804032304306, 1.000000000000000000, 0.9807852804032304306, 1.000000000000000000, 0.9807852804032304306, 1.000000000000000000, 0.9807852804032304306, 1.000000000000000000, 0.9807852804032304306, 1.000000000000000000, 0.9807852804032304306, 1.000000000000000000, 0.9807852804032302085, 1.000000000000000222 ) ) 
 REPRESENTATION_ITEM ( '' )  );
#5709 = CARTESIAN_POINT ( 'NONE',  ( -40.01497788969913216, 378.8073905601785327, 16.95518130045146776 ) ) ;
#5710 = ORIENTED_EDGE ( 'NONE', *, *, #14743, .T. ) ;
#5711 = CARTESIAN_POINT ( 'NONE',  ( -8.685887942688632180, 347.3073905765656377, -3.978247347592952732 ) ) ;
#5712 = VERTEX_POINT ( 'NONE', #5945 ) ;
#5713 = ORIENTED_EDGE ( 'NONE', *, *, #5129, .T. ) ;
#5714 = CARTESIAN_POINT ( 'NONE',  ( -44.16309181155858710, 515.9948905683720568, 6.410867750099241924 ) ) ;
#5715 = CARTESIAN_POINT ( 'NONE',  ( 6.416697501590670427, 217.7548513357008630, 60.00000000000000000 ) ) ;
#5716 = ORIENTED_EDGE ( 'NONE', *, *, #11380, .T. ) ;
#5717 = CARTESIAN_POINT ( 'NONE',  ( -11.93348319268871371, 300.6823905683720568, -3.332260488124732856 ) ) ;
#5718 = EDGE_LOOP ( 'NONE', ( #10263, #16298, #15111, #6585, #10764, #20245, #5688, #17006, #15049, #1552, #10951, #12239, #18301, #16188, #4756, #3569, #14815 ) ) ;
#5719 = CARTESIAN_POINT ( 'NONE',  ( -28.68588794268871212, 346.3698905683720568, 16.75240474999999307 ) ) ;
#5720 = CARTESIAN_POINT ( 'NONE',  ( -28.68588794268871212, 346.3698905683720568, 16.75240474999999307 ) ) ;
#5721 = EDGE_CURVE ( 'NONE', #5772, #4289, #2717, .T. ) ;
#5722 = CARTESIAN_POINT ( 'NONE',  ( -47.16347859291443712, 292.6198905765656377, 7.653668647301805628 ) ) ;
#5723 = CARTESIAN_POINT ( 'NONE',  ( -48.68588794268855224, 396.9323905601784759, -3.978247347593583783 ) ) ;
#5724 = CARTESIAN_POINT ( 'NONE',  ( -38.17536295476244135, 252.3073905683720284, -14.20200298773971426 ) ) ;
#5725 = FACE_OUTER_BOUND ( 'NONE', #3098, .T. ) ;
#5726 = CARTESIAN_POINT ( 'NONE',  ( -32.01814843081345430, 393.1823905683721136, -16.75240474999999307 ) ) ;
#5727 = DIRECTION ( 'NONE',  ( -1.000000000000000000, -0.000000000000000000, -0.000000000000000000 ) ) ;
#5728 = CARTESIAN_POINT ( 'NONE',  ( -8.685887942688555796, 447.3073905765654672, -3.978247347592740013 ) ) ;
#5729 = DIRECTION ( 'NONE',  ( 0.000000000000000000, 0.000000000000000000, -1.000000000000000000 ) ) ;
#5730 = EDGE_CURVE ( 'NONE', #4755, #15709, #12562, .T. ) ;
#5731 = CARTESIAN_POINT ( 'NONE',  ( -42.88789093042844769, 464.8073905683720568, 9.489475012073736337 ) ) ;
#5732 = EDGE_LOOP ( 'NONE', ( #19187, #7415, #20117, #17431 ) ) ;
#5733 = CARTESIAN_POINT ( 'NONE',  ( -10.20829729246299422, 441.6198905601784759, 7.653668647301790529 ) ) ;
#5734 = CARTESIAN_POINT ( 'NONE',  ( -13.20868407381884779, 278.2448905683720568, 6.410867750099229490 ) ) ;
#5735 = ORIENTED_EDGE ( 'NONE', *, *, #20130, .F. ) ;
#5736 = ORIENTED_EDGE ( 'NONE', *, *, #3454, .F. ) ;
#5737 = ORIENTED_EDGE ( 'NONE', *, *, #2893, .T. ) ;
#5738 = CARTESIAN_POINT ( 'NONE',  ( -43.68588794268869435, 213.9102039777116602, 0.000000000000000000 ) ) ;
#5739 = CARTESIAN_POINT ( 'NONE',  ( -28.68588794268870501, 296.3698905683720568, 16.75240474999999307 ) ) ;
#5740 = CARTESIAN_POINT ( 'NONE',  ( -19.19641293061497933, 368.8073905683720000, 14.20200298773971426 ) ) ;
#5741 = VECTOR ( 'NONE', #5205, 1000.000000000000227 ) ;
#5742 = CARTESIAN_POINT ( 'NONE',  ( 88.28695088269886071, 142.5259582928263455, 20.00000000000000355 ) ) ;
#5743 = CARTESIAN_POINT ( 'NONE',  ( -40.01497788969916058, 530.4323905765655809, -16.95518130045146421 ) ) ;
#5744 = CARTESIAN_POINT ( 'NONE',  ( -22.27502019258948351, 406.9948905683720000, 15.47720386886985189 ) ) ;
#5745 = CARTESIAN_POINT ( 'NONE',  ( -42.88789093042841927, 236.3073905683720284, 9.489475012073736337 ) ) ;
#5746 = CARTESIAN_POINT ( 'NONE',  ( -32.01814843081344719, 406.0573905683720000, 16.75240474999999307 ) ) ;
#5747 = ITEM_DEFINED_TRANSFORMATION ( 'NONE', 'NONE', #10367,  #12794 ) ;
#5748 = VECTOR ( 'NONE', #10439, 999.9999999999998863 ) ;
#5749 = CARTESIAN_POINT ( 'NONE',  ( -32.66413529028187668, 349.8073905765655809, -19.99999999999999289 ) ) ;
#5750 = DIRECTION ( 'NONE',  ( 0.000000000000000000, 0.000000000000000000, 1.000000000000000000 ) ) ;
#5751 = CARTESIAN_POINT ( 'NONE',  ( -28.68588794268870501, 306.3698905683720568, 16.75240474999999307 ) ) ;
#5752 = CARTESIAN_POINT ( 'NONE',  ( -40.53162694259545162, 464.1198905683720568, -11.84573899990672707 ) ) ;
#5753 = CARTESIAN_POINT ( 'NONE',  ( 20.42502041961814641, 160.1716627696692683, 40.00000000000000000 ) ) ;
#5754 = CARTESIAN_POINT ( 'NONE',  ( 27.98965548446208729, 333.8848358243226357, -40.00000000000000000 ) ) ;
#5755 = CARTESIAN_POINT ( 'NONE',  ( -28.68588794268874054, 573.2448905601785327, 0.000000000000000000 ) ) ;
#5756 = VECTOR ( 'NONE', #11081, 1000.000000000000000 ) ;
#5757 = CARTESIAN_POINT ( 'NONE',  ( -45.43829269268871229, 375.3698905683720568, 0.000000000000000000 ) ) ;
#5758 = CARTESIAN_POINT ( 'NONE',  ( -31.43925259815332041, 49.75942336920967790, -120.9825033997044557 ) ) ;
#5759 = CARTESIAN_POINT ( 'NONE',  ( -17.35679799567830983, 530.6823905601785327, 16.95518130045146421 ) ) ;
#5760 = CARTESIAN_POINT ( 'NONE',  ( -42.88789093042843348, 342.9323905683721136, -9.489475012073736337 ) ) ;
#5761 = VECTOR ( 'NONE', #15622, 1000.000000000000000 ) ;
#5762 = ORIENTED_EDGE ( 'NONE', *, *, #17681, .T. ) ;
#5763 = CARTESIAN_POINT ( 'NONE',  ( -22.27502019258950128, 510.7448905683720000, -15.47720386886985544 ) ) ;
#5764 = PRODUCT ( 'Heavy Perimeter Inertia Flywheel Disk', 'Heavy Perimeter Inertia Flywheel Disk', '', ( #5325 ) ) ;
#5765 = ORIENTED_EDGE ( 'NONE', *, *, #17085, .F. ) ;
#5766 = CARTESIAN_POINT ( 'NONE',  ( -21.03221929538692336, 354.1198905601785327, -18.47759065022572855 ) ) ;
#5767 = CARTESIAN_POINT ( 'NONE',  ( -38.86787825240671168, 223.9102039777116318, -13.30301237467029019 ) ) ;
#5768 = CARTESIAN_POINT ( 'NONE',  ( -45.64106924314017277, 312.9323905765655809, 11.32908994701042538 ) ) ;
#5769 = CARTESIAN_POINT ( 'NONE',  ( -71.26501780185373036, 213.9102039777116602, 25.00000000000000355 ) ) ;
#5770 = DIRECTION ( 'NONE',  ( -0.000000000000000000, -1.000000000000000000, -0.000000000000000000 ) ) ;
#5771 = CARTESIAN_POINT ( 'NONE',  ( -44.16309181155857999, 454.4948905683720568, 6.410867750099241924 ) ) ;
#5772 = VERTEX_POINT ( 'NONE', #11021 ) ;
#5773 = CARTESIAN_POINT ( 'NONE',  ( -13.20868407381887089, 468.2448905683720568, 6.410867750099229490 ) ) ;
#5774 = CARTESIAN_POINT ( 'NONE',  ( 32.47532367400565079, 600.7448905601785327, -163.9643442751439864 ) ) ;
#5775 = EDGE_CURVE ( 'NONE', #18006, #3567, #13504, .T. ) ;
#5776 = VECTOR ( 'NONE', #8163, 1000.000000000000000 ) ;
#5777 = CARTESIAN_POINT ( 'NONE',  ( -17.35679799567830273, 398.5573905765656377, -16.95518130045146421 ) ) ;
#5778 = DIRECTION ( 'NONE',  ( 1.000000000000000000, 0.000000000000000000, 0.000000000000000000 ) ) ;
#5779 = CARTESIAN_POINT ( 'NONE',  ( -14.54375231895775933, 300.9948905601784759, 14.14213562373094568 ) ) ;
#5780 = CARTESIAN_POINT ( 'NONE',  ( 0.4033376246892514949, -4.059728990630810941, -5.968343123267132455 ) ) ;
#5781 = CARTESIAN_POINT ( 'NONE',  ( -48.68588794268872277, 481.9948905765656377, 0.000000000000000000 ) ) ;
#5782 = EDGE_CURVE ( 'NONE', #10000, #11573, #19357, .T. ) ;
#5783 = EDGE_CURVE ( 'NONE', #19677, #14197, #1205, .T. ) ;
#5784 = CIRCLE ( 'NONE', #13033, 9.999999999999994671 ) ;
#5785 = DIRECTION ( 'NONE',  ( 1.000000000000000000, 0.000000000000000000, 0.000000000000000000 ) ) ;
#5786 = FACE_OUTER_BOUND ( 'NONE', #6502, .T. ) ;
#5787 = CARTESIAN_POINT ( 'NONE',  ( -40.53162694259543031, 276.6198905683720568, 11.84573899990672885 ) ) ;
#5788 = CARTESIAN_POINT ( 'NONE',  ( -48.68588794268869435, 256.9323905601784759, -3.978247347593158345 ) ) ;
#5789 = CARTESIAN_POINT ( 'NONE',  ( -11.73070664223724791, 366.0573905765656377, 11.32908994701042005 ) ) ;
#5790 = CARTESIAN_POINT ( 'NONE',  ( -35.09675569278795848, 437.2448905683720000, 15.47720386886985366 ) ) ;
#5791 = CARTESIAN_POINT ( 'NONE',  ( -42.82802356641965957, 330.7448905765655809, -14.14213562373094746 ) ) ;
#5792 = CARTESIAN_POINT ( 'NONE',  ( -25.35362745456396993, 268.1823905683720000, 16.75240474999998952 ) ) ;
#5793 = ADVANCED_FACE ( 'NONE', ( #2822 ), #1103, .T. ) ;
#5794 = VERTEX_POINT ( 'NONE', #11130 ) ;
#5795 = CARTESIAN_POINT ( 'NONE',  ( -28.68588794268872633, 378.8848358243226357, -38.00000000000000000 ) ) ;
#5796 = VERTEX_POINT ( 'NONE', #9508 ) ;
#5797 = CARTESIAN_POINT ( 'NONE',  ( -13.20868407381887621, 490.9948905683720568, -6.410867750099233042 ) ) ;
#5798 = VERTEX_POINT ( 'NONE', #18050 ) ;
#5799 = CARTESIAN_POINT ( 'NONE',  ( -28.68588794268873343, 524.4948905765655809, 19.99999999999999289 ) ) ;
#5800 = CARTESIAN_POINT ( 'NONE',  ( -40.53162694259542320, 235.1198905683720000, 11.84573899990672885 ) ) ;
#5801 = ORIENTED_EDGE ( 'NONE', *, *, #12746, .T. ) ;
#5802 = CARTESIAN_POINT ( 'NONE',  ( 51.50493485826542184, 170.1716627696692683, -57.52045949366692668 ) ) ;
#5803 = CARTESIAN_POINT ( 'NONE',  ( -47.16347859291445843, 472.6198905765656377, 7.653668647301805628 ) ) ;
#5804 = CARTESIAN_POINT ( 'NONE',  ( 0.2565376335220200255, -2.516992571281980950, 6.500000000000002665 ) ) ;
#5805 = CARTESIAN_POINT ( 'NONE',  ( -48.68588794268869435, 241.9948905765656377, 0.000000000000000000 ) ) ;
#5806 = LINE ( 'NONE', #858, #7723 ) ;
#5807 = CARTESIAN_POINT ( 'NONE',  ( -45.43829269268869808, 225.3698905683720284, 0.000000000000000000 ) ) ;
#5808 = CARTESIAN_POINT ( 'NONE',  ( -14.48388495494901740, 511.3073905683721136, -9.489475012073736337 ) ) ;
#5809 = CARTESIAN_POINT ( 'NONE',  ( 35.96497763894178945, 170.1716627696692683, 40.00000000000000000 ) ) ;
#5810 = CARTESIAN_POINT ( 'NONE',  ( -19.19641293061497223, 240.4323905683720284, -14.20200298773971603 ) ) ;
#5811 = CARTESIAN_POINT ( 'NONE',  ( -32.01814843081344719, 343.1823905683721136, -16.75240474999999307 ) ) ;
#5812 = CARTESIAN_POINT ( 'NONE',  ( -40.01497788969914637, 468.8073905601785327, 16.95518130045146776 ) ) ;
#5813 = CARTESIAN_POINT ( 'NONE',  ( -11.73070664223724613, 361.3073905601785327, 11.32908994701042005 ) ) ;
#5814 = CARTESIAN_POINT ( 'NONE',  ( -32.01814843081344719, 386.0573905683720000, 16.75240474999999307 ) ) ;
#5815 = CARTESIAN_POINT ( 'NONE',  ( -42.82802356641965247, 323.2448905765656377, 14.14213562373094923 ) ) ;
#5816 = CARTESIAN_POINT ( 'NONE',  ( -10.20829729246298712, 381.6198905601784759, 7.653668647301790529 ) ) ;
#5817 = VECTOR ( 'NONE', #19223, 1000.000000000000000 ) ;
#5818 = DIRECTION ( 'NONE',  ( 1.000000000000000000, 0.000000000000000000, 0.000000000000000000 ) ) ;
#5819 = EDGE_LOOP ( 'NONE', ( #17219, #13840, #8937, #1698 ) ) ;
#5820 = ORIENTED_EDGE ( 'NONE', *, *, #6980, .F. ) ;
#5821 = CARTESIAN_POINT ( 'NONE',  ( -19.19641293061500065, 501.9323905683720000, -14.20200298773971603 ) ) ;
#5822 = DIRECTION ( 'NONE',  ( 1.000000000000000000, 0.000000000000000000, 0.000000000000000000 ) ) ;
#5823 = ORIENTED_EDGE ( 'NONE', *, *, #7414, .F. ) ;
#5824 = CARTESIAN_POINT ( 'NONE',  ( -19.19641293061497223, 298.8073905683719431, 14.20200298773971426 ) ) ;
#5825 = VERTEX_POINT ( 'NONE', #11565 ) ;
#5826 = CARTESIAN_POINT ( 'NONE',  ( -42.88789093042843348, 334.8073905683720000, 9.489475012073736337 ) ) ;
#5827 = CARTESIAN_POINT ( 'NONE',  ( -44.16309181155857289, 343.2448905683720000, -6.410867750099231266 ) ) ;
#5828 = EDGE_CURVE ( 'NONE', #21078, #5342, #21104, .T. ) ;
#5829 = CARTESIAN_POINT ( 'NONE',  ( -48.68588794268870146, 281.6823905765656377, -3.978247347593158345 ) ) ;
#5830 = CARTESIAN_POINT ( 'NONE',  ( -32.66413529028187668, 395.0573905601784190, -19.99999999999999289 ) ) ;
#5831 = CARTESIAN_POINT ( 'NONE',  ( -22.27502019258947286, 250.7448905683720000, -15.47720386886985544 ) ) ;
#5832 = CARTESIAN_POINT ( 'NONE',  ( -40.01497788969914637, 463.5573905765655809, 16.95518130045146776 ) ) ;
#5833 = CARTESIAN_POINT ( 'NONE',  ( -11.93348319268872437, 390.3698905683720568, -2.051577885510841163E-15 ) ) ;
#5834 = VECTOR ( 'NONE', #4157, 1000.000000000000000 ) ;
#5835 = DIRECTION ( 'NONE',  ( -1.191790137725560488E-16, 1.000000000000000000, -0.000000000000000000 ) ) ;
#5836 = DIRECTION ( 'NONE',  ( -1.000000000000000000, 0.000000000000000000, 0.000000000000000000 ) ) ;
#5837 = B_SPLINE_CURVE_WITH_KNOTS ( 'NONE', 3,
 ( #11305, #3096, #8155, #1264, #4927, #1475, #6538, #19530, #1371, #14684, #21051, #4813, #12943, #2891, #19425, #12836, #1695, #11524 ),
 .UNSPECIFIED., .F., .F.,
 ( 4, 2, 2, 2, 2, 2, 2, 2, 4 ),
 ( 0.01574578602456869897, 0.01672957298347709301, 0.01771335994238548706, 0.01869714690129388110, 0.01968093386020227514, 0.02066472081911067266, 0.02164850777801906670, 0.02263229473692746074, 0.02361608169583585826 ),
 .UNSPECIFIED. ) ;
#5838 = ADVANCED_BREP_SHAPE_REPRESENTATION ( '', ( #11980, #12794 ), #12451 ) ;
#5839 =( BOUNDED_CURVE ( )  B_SPLINE_CURVE ( 2, ( #1980, #8552, #15172, #11108, #13064, #11220, #2909, #1494, #3008, #11323, #14590, #7754, #17712, #9490, #12743, #16319, #4625 ),
 .UNSPECIFIED., .F., .T. ) 
 B_SPLINE_CURVE_WITH_KNOTS ( ( 3, 2, 2, 2, 2, 2, 2, 2, 3 ),
 ( 0.4843750000000002220, 0.4863281250000002220, 0.4882812500000002220, 0.4902343750000002220, 0.4921875000000002220, 0.4941406250000002220, 0.4960937500000002220, 0.4980468750000002220, 0.5000000000000002220 ),
 .UNSPECIFIED. ) 
 CURVE ( )  GEOMETRIC_REPRESENTATION_ITEM ( )  RATIONAL_B_SPLINE_CURVE ( ( 0.9999999999999977796, 0.9807852804032326510, 1.000000000000000000, 0.9807852804032304306, 1.000000000000000000, 0.9807852804032304306, 1.000000000000000000, 0.9807852804032304306, 1.000000000000000000, 0.9807852804032304306, 1.000000000000000000, 0.9807852804032304306, 1.000000000000000000, 0.9807852804032304306, 1.000000000000000000, 0.9807852804032282101, 1.000000000000002220 ) ) 
 REPRESENTATION_ITEM ( '' )  );
#5840 = CARTESIAN_POINT ( 'NONE',  ( -46.31968306282883674, 160.1716627696692683, 33.59072564020503648 ) ) ;
#5841 = CARTESIAN_POINT ( 'NONE',  ( -45.43829269268871229, 444.1823905683719431, 3.332260488124734632 ) ) ;
#5842 = ORIENTED_EDGE ( 'NONE', *, *, #5178, .T. ) ;
#5843 = CARTESIAN_POINT ( 'NONE',  ( -10.20829729246299600, 442.8698905601784759, -7.653668647301794969 ) ) ;
#5844 = EDGE_CURVE ( 'NONE', #18480, #10315, #13859, .T. ) ;
#5845 = EDGE_LOOP ( 'NONE', ( #14172, #9672, #9254, #6479 ) ) ;
#5846 = CARTESIAN_POINT ( 'NONE',  ( -47.16347859291444422, 337.8698905601785327, 7.653668647301805628 ) ) ;
#5847 = ORIENTED_EDGE ( 'NONE', *, *, #18947, .F. ) ;
#5848 = ORIENTED_EDGE ( 'NONE', *, *, #1176, .T. ) ;
#5849 = CARTESIAN_POINT ( 'NONE',  ( 0.4042117618284690184, -3.141900367810046557, -6.499999999999999112 ) ) ;
#5850 = CARTESIAN_POINT ( 'NONE',  ( -42.82802356641965247, 318.4948905601784759, 14.14213562373094923 ) ) ;
#5851 = CARTESIAN_POINT ( 'NONE',  ( -42.88789093042842637, 294.8073905683720000, 9.489475012073736337 ) ) ;
#5852 = CIRCLE ( 'NONE', #13468, 20.00000000000000355 ) ;
#5853 = CARTESIAN_POINT ( 'NONE',  ( -22.27502019258948707, 362.2448905683720000, -15.47720386886985544 ) ) ;
#5854 = DIRECTION ( 'NONE',  ( -0.9365583756827543516, 0.000000000000000000, -0.3505116388060184329 ) ) ;
#5855 = FACE_OUTER_BOUND ( 'NONE', #10368, .T. ) ;
#5856 = CARTESIAN_POINT ( 'NONE',  ( -40.53162694259544452, 402.6198905683720568, -11.84573899990672707 ) ) ;
#5857 = CARTESIAN_POINT ( 'NONE',  ( -45.43829269268869098, 245.6823905683720284, 3.332260488124734632 ) ) ;
#5858 = CARTESIAN_POINT ( 'NONE',  ( -44.16309181155857999, 403.2448905683720568, -6.410867750099231266 ) ) ;
#5859 = AXIS2_PLACEMENT_3D ( 'NONE', #13578, #20167, #11934 ) ;
#5860 = ADVANCED_FACE ( 'NONE', ( #8310 ), #20755, .F. ) ;
#5861 = CARTESIAN_POINT ( 'NONE',  ( -47.16347859291444422, 342.6198905765656377, 7.653668647301805628 ) ) ;
#5862 = CARTESIAN_POINT ( 'NONE',  ( -8.685887942688717445, 322.2448905601784759, -2.449293598294705724E-15 ) ) ;
#5863 = CARTESIAN_POINT ( 'NONE',  ( -42.88789093042842637, 312.9323905683720000, -9.489475012073734561 ) ) ;
#5864 = CARTESIAN_POINT ( 'NONE',  ( -42.88789093042844769, 456.3073905683720000, 9.489475012073736337 ) ) ;
#5865 = CARTESIAN_POINT ( 'NONE',  ( -28.68588794268872277, 459.7448905601784759, 19.99999999999999289 ) ) ;
#5866 = CARTESIAN_POINT ( 'NONE',  ( -42.88696169552118675, 203.8418613323790396, -4.830328443944832628 ) ) ;
#5867 = DIRECTION ( 'NONE',  ( -0.4627175328665442677, 0.000000000000000000, -0.8865057725575725689 ) ) ;
#5868 = CARTESIAN_POINT ( 'NONE',  ( -19.19641293061498644, 371.9323905683720568, -14.20200298773971603 ) ) ;
#5869 = CARTESIAN_POINT ( 'NONE',  ( -11.93348319268873858, 499.1823905683720568, -3.332260488124732856 ) ) ;
#5870 = CARTESIAN_POINT ( 'NONE',  ( -14.54375231895778775, 513.4948905601785327, -14.14213562373094746 ) ) ;
#5871 = CARTESIAN_POINT ( 'NONE',  ( -28.68588794268870856, 336.3698905683720000, 16.75240474999999307 ) ) ;
#5872 = EDGE_CURVE ( 'NONE', #18587, #10793, #20002, .T. ) ;
#5873 = ORIENTED_EDGE ( 'NONE', *, *, #19748, .F. ) ;
#5874 = CARTESIAN_POINT ( 'NONE',  ( -35.09675569278796559, 495.7448905683720000, 15.47720386886985366 ) ) ;
#5875 = ORIENTED_EDGE ( 'NONE', *, *, #16648, .F. ) ;
#5876 = VECTOR ( 'NONE', #17356, 1000.000000000000000 ) ;
#5877 = DIRECTION ( 'NONE',  ( -1.000000000000000000, -0.000000000000000000, -0.000000000000000000 ) ) ;
#5878 = CARTESIAN_POINT ( 'NONE',  ( -11.93348319268872793, 420.6823905683720000, -3.332260488124732856 ) ) ;
#5879 = CARTESIAN_POINT ( 'NONE',  ( -17.35679799567828852, 288.5573905765655809, -16.95518130045146421 ) ) ;
#5880 = DIRECTION ( 'NONE',  ( 0.000000000000000000, 0.000000000000000000, 1.000000000000000000 ) ) ;
#5881 = CARTESIAN_POINT ( 'NONE',  ( -19.19641293061498999, 457.3073905683720568, 14.20200298773971426 ) ) ;
#5882 = EDGE_LOOP ( 'NONE', ( #15235, #6803, #2672, #14602 ) ) ;
#5883 = CARTESIAN_POINT ( 'NONE',  ( -11.93348319268873325, 459.1823905683720000, -3.332260488124732856 ) ) ;
#5884 = CARTESIAN_POINT ( 'NONE',  ( -47.16347859291443001, 247.8698905601785043, 7.653668647301805628 ) ) ;
#5885 = AXIS2_PLACEMENT_3D ( 'NONE', #16278, #12706, #2867 ) ;
#5886 = CARTESIAN_POINT ( 'NONE',  ( -17.35679799567830628, 408.5573905765655809, -16.95518130045146421 ) ) ;
#5887 = CARTESIAN_POINT ( 'NONE',  ( -8.685887942688536256, 277.3073905765655240, -3.978247347592740013 ) ) ;
#5888 = CARTESIAN_POINT ( 'NONE',  ( -48.68588794268854514, 371.6823905765655809, -3.978247347593583783 ) ) ;
#5889 = CARTESIAN_POINT ( 'NONE',  ( 5.074999999999999289, 7.505553499465139389, 0.000000000000000000 ) ) ;
#5890 = DIRECTION ( 'NONE',  ( 0.000000000000000000, 0.000000000000000000, -1.000000000000000000 ) ) ;
#5891 = CYLINDRICAL_SURFACE ( 'NONE', #10934, 4.000000000000001776 ) ;
#5892 = CIRCLE ( 'NONE', #17973, 5.000000000000004441 ) ;
#5893 = CARTESIAN_POINT ( 'NONE',  ( -32.66413529028187668, 435.0573905601784759, -19.99999999999999289 ) ) ;
#5894 = CARTESIAN_POINT ( 'NONE',  ( -10.20829729246298356, 342.8698905601785327, -7.653668647301794969 ) ) ;
#5895 = AXIS2_PLACEMENT_3D ( 'NONE', #4785, #17565, #2862 ) ;
#5896 = CARTESIAN_POINT ( 'NONE',  ( -22.27502019258946575, 278.4948905683720000, 15.47720386886985189 ) ) ;
#5897 = CARTESIAN_POINT ( 'NONE',  ( -8.685887942688708563, 252.5573905601784759, -3.978247347593165895 ) ) ;
#5898 = DIRECTION ( 'NONE',  ( 0.000000000000000000, 0.000000000000000000, 1.000000000000000000 ) ) ;
#5899 = CARTESIAN_POINT ( 'NONE',  ( -38.17536295476246266, 433.8073905683720568, -14.20200298773971426 ) ) ;
#5900 = CARTESIAN_POINT ( 'NONE',  ( -17.35679799567829917, 398.5573905765656377, -16.95518130045146421 ) ) ;
#5901 = CARTESIAN_POINT ( 'NONE',  ( -38.17536295476244135, 243.8073905683720284, -14.20200298773971426 ) ) ;
#5902 = ORIENTED_EDGE ( 'NONE', *, *, #5247, .T. ) ;
#5903 = PRODUCT_DEFINITION_FORMATION_WITH_SPECIFIED_SOURCE ( 'ANY', '', #7491, .NOT_KNOWN. ) ;
#5904 = CARTESIAN_POINT ( 'NONE',  ( -42.82802356641967378, 480.7448905765655809, -14.14213562373094746 ) ) ;
#5905 = ORIENTED_EDGE ( 'NONE', *, *, #18034, .F. ) ;
#5906 = CARTESIAN_POINT ( 'NONE',  ( -32.01814843081345430, 477.5573905683721136, 16.75240474999999307 ) ) ;
#5907 = VERTEX_POINT ( 'NONE', #9821 ) ;
#5908 = DIRECTION ( 'NONE',  ( 0.000000000000000000, 0.000000000000000000, 1.000000000000000000 ) ) ;
#5909 = CARTESIAN_POINT ( 'NONE',  ( -44.16309181155855867, 243.2448905683720000, -6.410867750099231266 ) ) ;
#5910 = ORIENTED_EDGE ( 'NONE', *, *, #12663, .T. ) ;
#5911 = CARTESIAN_POINT ( 'NONE',  ( -13.20868407381887977, 519.4948905683720568, -6.410867750099233042 ) ) ;
#5912 = LINE ( 'NONE', #16089, #12810 ) ;
#5913 = CARTESIAN_POINT ( 'NONE',  ( -40.01497788969915348, 460.4323905765656377, -16.95518130045146421 ) ) ;
#5914 = CARTESIAN_POINT ( 'NONE',  ( 20.42502041961813575, 271.1055109169419666, -20.00000000000000355 ) ) ;
#5915 = CARTESIAN_POINT ( 'NONE',  ( -48.68588794268855935, 456.9323905601784190, -3.978247347593583783 ) ) ;
#5916 = DIRECTION ( 'NONE',  ( 1.000000000000000000, 0.000000000000000000, -0.000000000000000000 ) ) ;
#5917 = VECTOR ( 'NONE', #11767, 1000.000000000000000 ) ;
#5918 = ADVANCED_FACE ( 'NONE', ( #5, #21297 ), #6469, .T. ) ;
#5919 = CARTESIAN_POINT ( 'NONE',  ( -16.84014894278200813, 511.6198905683720000, -11.84573899990672707 ) ) ;
#5920 = CARTESIAN_POINT ( 'NONE',  ( -21.03221929538691271, 375.1198905765656377, 18.47759065022572500 ) ) ;
#5921 = CARTESIAN_POINT ( 'NONE',  ( -42.88789093042841927, 252.9323905683720284, -9.489475012073736337 ) ) ;
#5922 = CARTESIAN_POINT ( 'NONE',  ( -11.93348319268871904, 330.0573905683720568, 3.332260488124728415 ) ) ;
#5923 = FACE_OUTER_BOUND ( 'NONE', #15443, .T. ) ;
#5924 = CARTESIAN_POINT ( 'NONE',  ( -28.68588794268870146, 274.4948905765656377, 19.99999999999999289 ) ) ;
#5925 = AXIS2_PLACEMENT_3D ( 'NONE', #9498, #13073, #21284 ) ;
#5926 = CARTESIAN_POINT ( 'NONE',  ( -40.53162694259543741, 385.1198905683720568, 11.84573899990672885 ) ) ;
#5927 = CARTESIAN_POINT ( 'NONE',  ( -10.20829729246298889, 392.8698905601784759, -7.653668647301794969 ) ) ;
#5928 = ORIENTED_EDGE ( 'NONE', *, *, #17501, .T. ) ;
#5929 = DIRECTION ( 'NONE',  ( 0.000000000000000000, -1.000000000000000000, 0.000000000000000000 ) ) ;
#5930 = VERTEX_POINT ( 'NONE', #16444 ) ;
#5931 = EDGE_LOOP ( 'NONE', ( #20762, #6890, #17178, #20655 ) ) ;
#5932 = CARTESIAN_POINT ( 'NONE',  ( -35.09675569278796559, 497.2448905683720000, 15.47720386886985366 ) ) ;
#5933 = DIRECTION ( 'NONE',  ( 0.000000000000000000, 0.000000000000000000, -1.000000000000000000 ) ) ;
#5934 = VERTEX_POINT ( 'NONE', #11344 ) ;
#5935 = CARTESIAN_POINT ( 'NONE',  ( -14.48388495494899075, 299.4323905683720568, 9.489475012073731008 ) ) ;
#5936 = ORIENTED_EDGE ( 'NONE', *, *, #1301, .T. ) ;
#5937 = CARTESIAN_POINT ( 'NONE',  ( -11.93348319268871727, 318.5573905683720000, 3.332260488124728415 ) ) ;
#5938 = VECTOR ( 'NONE', #4722, 1000.000000000000000 ) ;
#5939 = CARTESIAN_POINT ( 'NONE',  ( -45.43829269268871229, 353.5573905683721136, -3.332260488124726638 ) ) ;
#5940 = CARTESIAN_POINT ( 'NONE',  ( -21.03221929538690205, 275.1198905765655809, 18.47759065022572500 ) ) ;
#5941 = DIRECTION ( 'NONE',  ( 0.000000000000000000, 0.000000000000000000, -1.000000000000000000 ) ) ;
#5942 = CARTESIAN_POINT ( 'NONE',  ( -38.17536295476243424, 255.4323905683720284, 14.20200298773971781 ) ) ;
#5943 = CARTESIAN_POINT ( 'NONE',  ( -35.09675569278795138, 403.4948905683720000, -15.47720386886985544 ) ) ;
#5944 = CARTESIAN_POINT ( 'NONE',  ( 21.30000000000000071, 0.000000000000000000, 0.000000000000000000 ) ) ;
#5945 = CARTESIAN_POINT ( 'NONE',  ( 91.21585410611801592, 31.85652257517428865, -85.46735025547123143 ) ) ;
#5946 = PRODUCT ( 'MAS-323', 'MAS-323', '', ( #16810 ) ) ;
#5947 = CARTESIAN_POINT ( 'NONE',  ( -24.70764059509554755, 244.4323905601784475, -19.99999999999999289 ) ) ;
#5948 = CARTESIAN_POINT ( 'NONE',  ( -14.48388495494900852, 449.8073905683720000, -9.489475012073736337 ) ) ;
#5949 = ORIENTED_EDGE ( 'NONE', *, *, #16507, .F. ) ;
#5950 = VECTOR ( 'NONE', #17223, 999.9999999999998863 ) ;
#5951 = CARTESIAN_POINT ( 'NONE',  ( -47.16347859291445133, 447.8698905601785327, 7.653668647301805628 ) ) ;
#5952 = ORIENTED_EDGE ( 'NONE', *, *, #7317, .F. ) ;
#5953 = ORIENTED_EDGE ( 'NONE', *, *, #2699, .F. ) ;
#5954 = EDGE_LOOP ( 'NONE', ( #15319, #14835, #8075, #16484 ) ) ;
#5955 = CARTESIAN_POINT ( 'NONE',  ( 162.8695233526006803, 610.7448905601785327, -10.81142786866620575 ) ) ;
#5956 = CARTESIAN_POINT ( 'NONE',  ( -32.66413529028186957, 319.4323905601785327, 19.99999999999999289 ) ) ;
#5957 = EDGE_CURVE ( 'NONE', #14447, #13267, #14832, .T. ) ;
#5958 = CARTESIAN_POINT ( 'NONE',  ( -28.68588794268871567, 362.8698905683720000, -16.75240474999999307 ) ) ;
#5959 = FACE_OUTER_BOUND ( 'NONE', #12594, .T. ) ;
#5960 = EDGE_CURVE ( 'NONE', #4339, #14946, #5892, .T. ) ;
#5961 = CARTESIAN_POINT ( 'NONE',  ( -10.20829729246300310, 507.6198905765656377, -7.653668647301794969 ) ) ;
#5962 = CARTESIAN_POINT ( 'NONE',  ( -11.93348319268872615, 408.5573905683720568, 3.332260488124728415 ) ) ;
#5963 = CARTESIAN_POINT ( 'NONE',  ( -16.84014894278197261, 239.1198905683720284, 11.84573899990672530 ) ) ;
#5964 = VECTOR ( 'NONE', #10008, 1000.000000000000114 ) ;
#5965 = CARTESIAN_POINT ( 'NONE',  ( -38.17536295476245556, 415.4323905683721136, 14.20200298773971781 ) ) ;
#5966 = CARTESIAN_POINT ( 'NONE',  ( -40.01497788969913927, 340.4323905765656946, -16.95518130045146421 ) ) ;
#5967 = CARTESIAN_POINT ( 'NONE',  ( -14.54375231895776466, 323.4948905601784759, -14.14213562373094746 ) ) ;
#5968 = CARTESIAN_POINT ( 'NONE',  ( -45.43829269268870519, 303.5573905683720568, -3.332260488124726638 ) ) ;
#5969 =( NAMED_UNIT ( * ) PLANE_ANGLE_UNIT ( ) SI_UNIT ( $, .RADIAN. ) );
#5970 =( BOUNDED_CURVE ( )  B_SPLINE_CURVE ( 2, ( #67, #5018, #11726, #6744, #11618, #175, #3508, #16396, #6849, #5127, #13360, #19730, #11509, #10198, #9770, #1797, #3301 ),
 .UNSPECIFIED., .F., .T. ) 
 B_SPLINE_CURVE_WITH_KNOTS ( ( 3, 2, 2, 2, 2, 2, 2, 2, 3 ),
 ( 0.2187500000000001943, 0.2207031250000001943, 0.2226562500000001943, 0.2246093750000001943, 0.2265625000000001943, 0.2285156250000001943, 0.2304687500000001943, 0.2324218750000001943, 0.2343750000000001943 ),
 .UNSPECIFIED. ) 
 CURVE ( )  GEOMETRIC_REPRESENTATION_ITEM ( )  RATIONAL_B_SPLINE_CURVE ( ( 0.9999999999999981126, 0.9807852804032323180, 1.000000000000000000, 0.9807852804032304306, 1.000000000000000000, 0.9807852804032304306, 1.000000000000000000, 0.9807852804032304306, 1.000000000000000000, 0.9807852804032304306, 1.000000000000000000, 0.9807852804032304306, 1.000000000000000000, 0.9807852804032304306, 1.000000000000000000, 0.9807852804032285432, 1.000000000000001998 ) ) 
 REPRESENTATION_ITEM ( '' )  );
#5971 = CARTESIAN_POINT ( 'NONE',  ( -35.09675569278796559, 457.2448905683720568, 15.47720386886985366 ) ) ;
#5972 = CARTESIAN_POINT ( 'NONE',  ( -36.33955658999052929, 459.1198905601784759, 18.47759065022572500 ) ) ;
#5973 = CARTESIAN_POINT ( 'NONE',  ( 0.000000000000000000, 5.629165124598846326, -3.250000000000007550 ) ) ;
#5974 = CARTESIAN_POINT ( 'NONE',  ( 158.8141120573112630, 400.5398297725603243, 0.000000000000000000 ) ) ;
#5975 = CIRCLE ( 'NONE', #19457, 4.000000000000001776 ) ;
#5976 = CARTESIAN_POINT ( 'NONE',  ( -14.48388495494899963, 361.3073905683721136, -9.489475012073736337 ) ) ;
#5977 = CARTESIAN_POINT ( 'NONE',  ( -11.93348319268873858, 509.1823905683719431, -3.332260488124732856 ) ) ;
#5978 =( REPRESENTATION_RELATIONSHIP ('NONE','NONE', #1888, #15840 ) REPRESENTATION_RELATIONSHIP_WITH_TRANSFORMATION ( #5747 )SHAPE_REPRESENTATION_RELATIONSHIP( ) );
#5979 = AXIS2_PLACEMENT_3D ( 'NONE', #19567, #1517, #11566 ) ;
#5980 = CARTESIAN_POINT ( 'NONE',  ( -11.73070664223726389, 511.3073905601785327, 11.32908994701042005 ) ) ;
#5981 = CARTESIAN_POINT ( 'NONE',  ( -42.88789093042842637, 322.9323905683720000, -9.489475012073736337 ) ) ;
#5982 = EDGE_CURVE ( 'NONE', #13870, #264, #6690, .T. ) ;
#5983 = ORIENTED_EDGE ( 'NONE', *, *, #11593, .T. ) ;
#5984 = CARTESIAN_POINT ( 'NONE',  ( -45.43829269268871940, 503.5573905683720000, -3.332260488124726194 ) ) ;
#5985 = VERTEX_POINT ( 'NONE', #6795 ) ;
#5986 = CARTESIAN_POINT ( 'NONE',  ( -8.685887942688720997, 352.2448905601784759, -2.449293598294705724E-15 ) ) ;
#5987 = CARTESIAN_POINT ( 'NONE',  ( -11.93348319268872793, 420.0573905683720000, 3.332260488124728859 ) ) ;
#5988 = CARTESIAN_POINT ( 'NONE',  ( -40.01497788969913927, 393.5573905765655809, 16.95518130045146776 ) ) ;
#5989 = FILL_AREA_STYLE ('',( #10956 ) ) ;
#5990 = CARTESIAN_POINT ( 'NONE',  ( -44.16309181155858710, 463.2448905683720568, -6.410867750099231266 ) ) ;
#5991 = ORIENTED_EDGE ( 'NONE', *, *, #2055, .T. ) ;
#5992 = CARTESIAN_POINT ( 'NONE',  ( -25.35362745456399125, 456.6823905683720000, 16.75240474999998952 ) ) ;
#5993 = CARTESIAN_POINT ( 'NONE',  ( -11.73070664223723192, 251.3073905601784759, 11.32908994701042005 ) ) ;
#5994 = AXIS2_PLACEMENT_3D ( 'NONE', #15230, #13502, #6990 ) ;
#5995 = CARTESIAN_POINT ( 'NONE',  ( -17.35679799567829917, 405.4323905765655240, 16.95518130045146421 ) ) ;
#5996 = CARTESIAN_POINT ( 'NONE',  ( -20.54277306141298354, 600.7448905601785327, -49.33244044267773631 ) ) ;
#5997 = CARTESIAN_POINT ( 'NONE',  ( -28.68588794268875120, 610.7448905601785327, 0.000000000000000000 ) ) ;
#5998 = CARTESIAN_POINT ( 'NONE',  ( 5.299999999999999822, 0.000000000000000000, 0.000000000000000000 ) ) ;
#5999 = DIRECTION ( 'NONE',  ( 0.000000000000000000, -1.000000000000000000, 0.000000000000000000 ) ) ;
#6000 = VECTOR ( 'NONE', #12385, 1000.000000000000000 ) ;
#6001 = ADVANCED_FACE ( 'NONE', ( #16232 ), #13413, .F. ) ;
#6002 = DIRECTION ( 'NONE',  ( -0.3505116388060184329, 0.000000000000000000, -0.9365583756827543516 ) ) ;
#6003 = CARTESIAN_POINT ( 'NONE',  ( -43.91866333689311830, 223.9102039777115749, 10.20022563105532676 ) ) ;
#6004 = CARTESIAN_POINT ( 'NONE',  ( -17.35679799567828496, 243.8073905601784475, -16.95518130045146421 ) ) ;
#6005 = CARTESIAN_POINT ( 'NONE',  ( -14.54375231895776821, 365.7448905765656377, 14.14213562373094568 ) ) ;
#6006 = CARTESIAN_POINT ( 'NONE',  ( -32.01814843081345430, 433.1823905683721136, -16.75240474999999307 ) ) ;
#6007 = LINE ( 'NONE', #6108, #5401 ) ;
#6008 = CARTESIAN_POINT ( 'NONE',  ( -45.43829269268869098, 255.6823905683720000, 3.332260488124734632 ) ) ;
#6009 = EDGE_CURVE ( 'NONE', #9261, #5794, #19811, .T. ) ;
#6010 = ORIENTED_EDGE ( 'NONE', *, *, #7435, .T. ) ;
#6011 = VERTEX_POINT ( 'NONE', #14756 ) ;
#6012 = DIRECTION ( 'NONE',  ( -1.000000000000000000, -1.191790137725560488E-16, 0.000000000000000000 ) ) ;
#6013 = ORIENTED_EDGE ( 'NONE', *, *, #6841, .T. ) ;
#6014 = CARTESIAN_POINT ( 'NONE',  ( -14.48388495494901029, 461.3073905683720568, -9.489475012073734561 ) ) ;
#6015 = ORIENTED_EDGE ( 'NONE', *, *, #11793, .F. ) ;
#6016 = LINE ( 'NONE', #7309, #4852 ) ;
#6017 = CARTESIAN_POINT ( 'NONE',  ( -40.53162694259542320, 242.6198905683720284, -11.84573899990672707 ) ) ;
#6018 = ORIENTED_EDGE ( 'NONE', *, *, #12630, .T. ) ;
#6019 = CARTESIAN_POINT ( 'NONE',  ( -11.93348319268874036, 518.8698905683719431, -2.051577885510841163E-15 ) ) ;
#6020 = LINE ( 'NONE', #7419, #4171 ) ;
#6021 = CARTESIAN_POINT ( 'NONE',  ( -48.68588794268872277, 461.6823905765656377, -3.978247347593158345 ) ) ;
#6022 = FACE_BOUND ( 'NONE', #20993, .T. ) ;
#6023 = CARTESIAN_POINT ( 'NONE',  ( -21.03221929538690205, 285.1198905765656377, 18.47759065022572500 ) ) ;
#6024 = CARTESIAN_POINT ( 'NONE',  ( -35.32494336579074456, 223.9102039777116602, -16.19735568274630921 ) ) ;
#6025 = CARTESIAN_POINT ( 'NONE',  ( -13.20868407381884424, 229.7448905683720568, 6.410867750099229490 ) ) ;
#6026 = LINE ( 'NONE', #19124, #18384 ) ;
#6027 = CARTESIAN_POINT ( 'NONE',  ( -21.25396403206155682, 220.6412462828192247, -15.05426855923459328 ) ) ;
#6028 = CARTESIAN_POINT ( 'NONE',  ( -25.35362745456398770, 332.5573905683720000, -16.75240474999999307 ) ) ;
#6029 = DIRECTION ( 'NONE',  ( 0.000000000000000000, 0.000000000000000000, 1.000000000000000000 ) ) ;
#6030 = CARTESIAN_POINT ( 'NONE',  ( -40.53162694259543031, 314.1198905683720568, -11.84573899990672707 ) ) ;
#6031 = CARTESIAN_POINT ( 'NONE',  ( -38.17536295476245556, 382.3073905683719431, -14.20200298773971426 ) ) ;
#6032 = CARTESIAN_POINT ( 'NONE',  ( -38.17536295476246977, 526.9323905683720568, 14.20200298773971781 ) ) ;
#6033 = EDGE_CURVE ( 'NONE', #3667, #20822, #18879, .T. ) ;
#6034 = CARTESIAN_POINT ( 'NONE',  ( -48.68588794268870856, 387.5573905601784759, 3.978247347593168115 ) ) ;
#6035 = EDGE_CURVE ( 'NONE', #5798, #10333, #6082, .T. ) ;
#6036 = CARTESIAN_POINT ( 'NONE',  ( 32.47532367400570052, 600.7448905601785327, 163.9643442751439011 ) ) ;
#6037 = ORIENTED_EDGE ( 'NONE', *, *, #2836, .F. ) ;
#6038 = VERTEX_POINT ( 'NONE', #11054 ) ;
#6039 = CARTESIAN_POINT ( 'NONE',  ( -14.48388495494901740, 511.3073905683721136, -9.489475012073736337 ) ) ;
#6040 = LINE ( 'NONE', #12323, #424 ) ;
#6041 = EDGE_LOOP ( 'NONE', ( #15712, #9599, #287, #11628 ) ) ;
#6042 = CARTESIAN_POINT ( 'NONE',  ( -25.35362745456397349, 308.1823905683719431, 16.75240474999998952 ) ) ;
#6043 = CARTESIAN_POINT ( 'NONE',  ( -35.09675569278793716, 321.9948905683720568, -15.47720386886985544 ) ) ;
#6044 = EDGE_CURVE ( 'NONE', #14946, #4339, #6917, .T. ) ;
#6045 = CARTESIAN_POINT ( 'NONE',  ( -17.35679799567828852, 258.5573905765655809, -16.95518130045146421 ) ) ;
#6046 = CARTESIAN_POINT ( 'NONE',  ( -48.68588794268871567, 397.2448905601784759, 0.000000000000000000 ) ) ;
#6047 = CARTESIAN_POINT ( 'NONE',  ( -25.35362745456396638, 236.6823905683720284, 16.75240474999998952 ) ) ;
#6048 = EDGE_CURVE ( 'NONE', #4866, #15132, #623, .T. ) ;
#6049 = CARTESIAN_POINT ( 'NONE',  ( -28.68588794268871922, 402.8698905683720000, -16.75240474999999307 ) ) ;
#6050 = EDGE_CURVE ( 'NONE', #14751, #15077, #11490, .T. ) ;
#6051 = DIRECTION ( 'NONE',  ( -1.000000000000000000, -0.000000000000000000, -0.000000000000000000 ) ) ;
#6052 = FACE_OUTER_BOUND ( 'NONE', #5027, .T. ) ;
#6053 = CARTESIAN_POINT ( 'NONE',  ( -24.70764059509557597, 509.1823905765655809, -19.99999999999999289 ) ) ;
#6054 = CARTESIAN_POINT ( 'NONE',  ( -40.53162694259544452, 435.1198905683720000, 11.84573899990672885 ) ) ;
#6055 = ORIENTED_EDGE ( 'NONE', *, *, #560, .F. ) ;
#6056 = CARTESIAN_POINT ( 'NONE',  ( -8.685887942688729879, 442.2448905601785327, -2.449293598294705724E-15 ) ) ;
#6057 = EDGE_CURVE ( 'NONE', #5712, #5798, #1136, .T. ) ;
#6058 = ORIENTED_EDGE ( 'NONE', *, *, #17304, .T. ) ;
#6059 = ORIENTED_EDGE ( 'NONE', *, *, #14317, .T. ) ;
#6060 = VERTEX_POINT ( 'NONE', #8018 ) ;
#6061 = CYLINDRICAL_SURFACE ( 'NONE', #21155, 19.99999999999999645 ) ;
#6062 = CARTESIAN_POINT ( 'NONE',  ( -47.16347859291443712, 327.8698905601785327, 7.653668647301805628 ) ) ;
#6063 = CARTESIAN_POINT ( 'NONE',  ( -42.88789093042843348, 356.3073905683720000, 9.489475012073734561 ) ) ;
#6064 = CYLINDRICAL_SURFACE ( 'NONE', #3135, 19.99999999999999645 ) ;
#6065 = CARTESIAN_POINT ( 'NONE',  ( -21.03221929538694113, 498.8698905765656377, -18.47759065022572855 ) ) ;
#6066 = CARTESIAN_POINT ( 'NONE',  ( -45.43829269268871940, 393.8698905683720000, 0.000000000000000000 ) ) ;
#6067 = CARTESIAN_POINT ( 'NONE',  ( -45.43829269268869098, 235.6823905683720284, 3.332260488124734632 ) ) ;
#6068 = CARTESIAN_POINT ( 'NONE',  ( -11.93348319268872615, 408.8698905683720568, -2.051577885510841163E-15 ) ) ;
#6069 = CARTESIAN_POINT ( 'NONE',  ( -45.64106924314017988, 321.0573905765656377, -11.32908994701042715 ) ) ;
#6070 = DIRECTION ( 'NONE',  ( -0.000000000000000000, -0.000000000000000000, -1.000000000000000000 ) ) ;
#6071 = CARTESIAN_POINT ( 'NONE',  ( -19.19641293061497578, 300.4323905683720568, -14.20200298773971603 ) ) ;
#6072 = CARTESIAN_POINT ( 'NONE',  ( -16.84014894278199748, 449.1198905683720568, 11.84573899990672530 ) ) ;
#6073 = CARTESIAN_POINT ( 'NONE',  ( -54.57497958038185004, 230.5765313837437418, 49.99999999999999289 ) ) ;
#6074 = CARTESIAN_POINT ( 'NONE',  ( -28.68588794268871212, 369.7448905601785327, 19.99999999999999289 ) ) ;
#6075 = CARTESIAN_POINT ( 'NONE',  ( -8.685887942688729879, 432.2448905601785327, -2.449293598294705724E-15 ) ) ;
#6076 = CARTESIAN_POINT ( 'NONE',  ( -19.19641293061498288, 358.8073905683720000, 14.20200298773971426 ) ) ;
#6077 = CARTESIAN_POINT ( 'NONE',  ( -45.43829269268871940, 494.1823905683720000, 3.332260488124734632 ) ) ;
#6078 = CARTESIAN_POINT ( 'NONE',  ( -11.73070664223726745, 503.1823905601785327, -11.32908994701042715 ) ) ;
#6079 = CARTESIAN_POINT ( 'NONE',  ( -32.01814843081344719, 331.6823905683720000, -16.75240474999999307 ) ) ;
#6080 = AXIS2_PLACEMENT_3D ( 'NONE', #4884, #6821, #13226 ) ;
#6081 = EDGE_LOOP ( 'NONE', ( #19533, #7304 ) ) ;
#6082 = LINE ( 'NONE', #17871, #16268 ) ;
#6083 = ORIENTED_EDGE ( 'NONE', *, *, #15630, .F. ) ;
#6084 = LINE ( 'NONE', #7493, #20518 ) ;
#6085 = CIRCLE ( 'NONE', #14408, 21.20245194746113526 ) ;
#6086 = CARTESIAN_POINT ( 'NONE',  ( -32.01814843081344719, 423.1823905683721136, -16.75240474999999307 ) ) ;
#6087 = CARTESIAN_POINT ( 'NONE',  ( -42.82802356641964536, 233.2448905765656093, 14.14213562373094923 ) ) ;
#6088 = FACE_OUTER_BOUND ( 'NONE', #20327, .T. ) ;
#6089 = CARTESIAN_POINT ( 'NONE',  ( -14.48388495494900852, 439.8073905683721136, -9.489475012073736337 ) ) ;
#6090 = EDGE_LOOP ( 'NONE', ( #12126, #2830, #7840, #1745 ) ) ;
#6091 = CARTESIAN_POINT ( 'NONE',  ( -45.43829269268872650, 474.1823905683720000, 3.332260488124734632 ) ) ;
#6092 = CARTESIAN_POINT ( 'NONE',  ( -21.03221929538693047, 414.1198905601785327, -18.47759065022572855 ) ) ;
#6093 = CARTESIAN_POINT ( 'NONE',  ( -21.03221929538693047, 408.8698905765656377, -18.47759065022572855 ) ) ;
#6094 = LINE ( 'NONE', #12499, #21382 ) ;
#6095 = CYLINDRICAL_SURFACE ( 'NONE', #11652, 200.0000000000000000 ) ;
#6096 = CARTESIAN_POINT ( 'NONE',  ( 0.05533025579362596535, -4.993776679985865385, -4.350525068611872825 ) ) ;
#6097 = DIRECTION ( 'NONE',  ( 1.000000000000000000, 0.000000000000000000, 0.000000000000000000 ) ) ;
#6098 = ADVANCED_FACE ( 'NONE', ( #14650 ), #9754, .F. ) ;
#6099 = CIRCLE ( 'NONE', #956, 9.999999999999994671 ) ;
#6100 = FACE_OUTER_BOUND ( 'NONE', #5610, .T. ) ;
#6101 = DIRECTION ( 'NONE',  ( -1.191790137725560488E-16, 1.000000000000000000, -0.000000000000000000 ) ) ;
#6102 = CARTESIAN_POINT ( 'NONE',  ( -47.16347859291444422, 346.6198905601784190, -7.653668647301793193 ) ) ;
#6103 = APPLICATION_CONTEXT ( 'automotive_design' ) ;
#6104 = CARTESIAN_POINT ( 'NONE',  ( -28.68588794268869790, 239.7448905601785043, 19.99999999999999289 ) ) ;
#6105 = CIRCLE ( 'NONE', #1286, 43.46661168214937732 ) ;
#6106 = CARTESIAN_POINT ( 'NONE',  ( -8.685887942688911068, 451.9323905601784759, 3.978247347593586447 ) ) ;
#6107 = CARTESIAN_POINT ( 'NONE',  ( -14.48388495494900674, 431.3073905683719431, -9.489475012073736337 ) ) ;
#6108 = CARTESIAN_POINT ( 'NONE',  ( -49.57497958038185715, 160.1716627696692683, 50.00000000000000000 ) ) ;
#6109 = CARTESIAN_POINT ( 'NONE',  ( -25.35362745456397704, 252.5573905683720284, -16.75240474999999307 ) ) ;
#6110 = VERTEX_POINT ( 'NONE', #11377 ) ;
#6111 = ORIENTED_EDGE ( 'NONE', *, *, #15232, .T. ) ;
#6112 = CARTESIAN_POINT ( 'NONE',  ( -45.64106924314018698, 422.9323905765656946, 11.32908994701042538 ) ) ;
#6113 = ORIENTED_EDGE ( 'NONE', *, *, #13198, .T. ) ;
#6114 = CARTESIAN_POINT ( 'NONE',  ( -45.43829269268872650, 465.6823905683720000, 3.332260488124734632 ) ) ;
#6115 = CARTESIAN_POINT ( 'NONE',  ( -36.33955658999050087, 233.8698905765656093, 18.47759065022572500 ) ) ;
#6116 = EDGE_CURVE ( 'NONE', #5342, #12399, #20061, .T. ) ;
#6117 = AXIS2_PLACEMENT_3D ( 'NONE', #20052, #3608, #10193 ) ;
#6118 = VERTEX_POINT ( 'NONE', #18405 ) ;
#6119 = DIRECTION ( 'NONE',  ( 1.232945044042657126E-32, -9.855701800883825964E-17, 1.000000000000000000 ) ) ;
#6120 = CARTESIAN_POINT ( 'NONE',  ( -22.27502019258947286, 230.7448905683720000, -15.47720386886985544 ) ) ;
#6121 = EDGE_LOOP ( 'NONE', ( #15052, #21157, #12224, #6055 ) ) ;
#6122 = CARTESIAN_POINT ( 'NONE',  ( -45.43829269268873361, 533.5573905683720568, -3.332260488124726638 ) ) ;
#6123 = DIRECTION ( 'NONE',  ( 0.000000000000000000, 0.000000000000000000, -1.000000000000000000 ) ) ;
#6124 = CARTESIAN_POINT ( 'NONE',  ( -14.54375231895777887, 465.7448905765655809, 14.14213562373094568 ) ) ;
#6125 = PRODUCT_DEFINITION_SHAPE ( 'NONE', 'NONE',  #4341 ) ;
#6126 = CARTESIAN_POINT ( 'NONE',  ( -28.68588794268872633, 250.8848358243226357, 0.000000000000000000 ) ) ;
#6127 = LINE ( 'NONE', #12412, #11150 ) ;
#6128 = CARTESIAN_POINT ( 'NONE',  ( -174.5421710038924346, 600.7448905601785327, -96.70028278950395872 ) ) ;
#6129 = CARTESIAN_POINT ( 'NONE',  ( -14.48388495494898365, 231.3073905683720284, -9.489475012073734561 ) ) ;
#6130 = EDGE_CURVE ( 'NONE', #12049, #11027, #17096, .T. ) ;
#6131 = CARTESIAN_POINT ( 'NONE',  ( -8.882341142746135176, 223.9102039777117454, 3.228969530591021098 ) ) ;
#6132 = CARTESIAN_POINT ( 'NONE',  ( -44.16309181155855157, 224.4948905683720284, 6.410867750099241924 ) ) ;
#6133 = CARTESIAN_POINT ( 'NONE',  ( -13.20868407381885490, 310.9948905683720568, -6.410867750099233042 ) ) ;
#6134 = CARTESIAN_POINT ( 'NONE',  ( -42.82802356641966668, 445.9948905601784759, -14.14213562373094746 ) ) ;
#6135 = CARTESIAN_POINT ( 'NONE',  ( 0.5805565836007611225, 3.752776749732563033, 6.500000000000000000 ) ) ;
#6136 = CARTESIAN_POINT ( 'NONE',  ( -14.48388495494899253, 301.3073905683720568, -9.489475012073736337 ) ) ;
#6137 = CARTESIAN_POINT ( 'NONE',  ( -44.16309181155857289, 383.2448905683720000, -6.410867750099231266 ) ) ;
#6138 = CARTESIAN_POINT ( 'NONE',  ( -11.93348319268874036, 520.0573905683719431, 3.332260488124728859 ) ) ;
#6139 = CARTESIAN_POINT ( 'NONE',  ( -24.70764059509556532, 394.4323905601784190, -19.99999999999999289 ) ) ;
#6140 = CARTESIAN_POINT ( 'NONE',  ( -36.33955658999049376, 230.1198905765656093, -18.47759065022572855 ) ) ;
#6141 = ORIENTED_EDGE ( 'NONE', *, *, #5457, .T. ) ;
#6142 = ORIENTED_EDGE ( 'NONE', *, *, #13800, .T. ) ;
#6143 = CARTESIAN_POINT ( 'NONE',  ( -14.48388495494901562, 491.3073905683720000, -9.489475012073736337 ) ) ;
#6144 = DIRECTION ( 'NONE',  ( 1.000000000000000000, 0.000000000000000000, 0.000000000000000000 ) ) ;
#6145 = VERTEX_POINT ( 'NONE', #3283 ) ;
#6146 = CARTESIAN_POINT ( 'NONE',  ( -22.27502019258946930, 288.4948905683720000, 15.47720386886985189 ) ) ;
#6147 = CARTESIAN_POINT ( 'NONE',  ( -11.93348319268871904, 328.5573905683720568, 3.332260488124728415 ) ) ;
#6148 = CARTESIAN_POINT ( 'NONE',  ( -14.54375231895775578, 265.7448905765656377, 14.14213562373094568 ) ) ;
#6149 = CARTESIAN_POINT ( 'NONE',  ( 18.55315245287936321, 213.9102039777116602, -25.00000000000000000 ) ) ;
#6150 = CARTESIAN_POINT ( 'NONE',  ( 71.32175588950862277, 75.31183677523708297, 94.99999999999994316 ) ) ;
#6151 = CARTESIAN_POINT ( 'NONE',  ( -32.01814843081344719, 373.1823905683720000, -16.75240474999999307 ) ) ;
#6152 = CARTESIAN_POINT ( 'NONE',  ( -42.83951137863823533, 204.4886979175576016, 4.967857365464206865 ) ) ;
#6153 = DIRECTION ( 'NONE',  ( -1.000000000000000000, 0.000000000000000000, 0.000000000000000000 ) ) ;
#6154 = CARTESIAN_POINT ( 'NONE',  ( -8.685887942688742314, 573.2448905601785327, 2.449293598294706119E-15 ) ) ;
#6155 = CIRCLE ( 'NONE', #4438, 175.0000000000000284 ) ;
#6156 = CARTESIAN_POINT ( 'NONE',  ( -40.53162694259544452, 442.6198905683720568, -11.84573899990672707 ) ) ;
#6157 = CARTESIAN_POINT ( 'NONE',  ( 6.416697501590670427, 217.7548513357008630, 45.00000000000000000 ) ) ;
#6158 = ORIENTED_EDGE ( 'NONE', *, *, #3412, .T. ) ;
#6159 = CARTESIAN_POINT ( 'NONE',  ( -40.01497788969914637, 445.6823905601784759, -16.95518130045146421 ) ) ;
#6160 = EDGE_CURVE ( 'NONE', #9040, #13902, #12488, .T. ) ;
#6161 = ORIENTED_EDGE ( 'NONE', *, *, #21293, .F. ) ;
#6162 = VERTEX_POINT ( 'NONE', #18088 ) ;
#6163 = PLANE ( 'NONE',  #3540 ) ;
#6164 = CARTESIAN_POINT ( 'NONE',  ( -14.54375231895776288, 330.9948905601784190, 14.14213562373094568 ) ) ;
#6165 = CARTESIAN_POINT ( 'NONE',  ( -10.20829729246298712, 377.6198905765655809, -7.653668647301794969 ) ) ;
#6166 = EDGE_CURVE ( 'NONE', #16379, #18572, #19797, .T. ) ;
#6167 = EDGE_CURVE ( 'NONE', #15709, #20838, #6614, .T. ) ;
#6168 = ADVANCED_FACE ( 'NONE', ( #42 ), #15180, .F. ) ;
#6169 = CARTESIAN_POINT ( 'NONE',  ( -45.43829269268871229, 365.3698905683720568, 0.000000000000000000 ) ) ;
#6170 = CARTESIAN_POINT ( 'NONE',  ( -48.68588794268878672, 227.5573905601784475, 3.978247347592954952 ) ) ;
#6171 = CARTESIAN_POINT ( 'NONE',  ( -45.64106924314020119, 502.9323905765656946, 11.32908994701042715 ) ) ;
#6172 = CARTESIAN_POINT ( 'NONE',  ( -11.93348319268872260, 378.5573905683721136, 3.332260488124728415 ) ) ;
#6173 = CARTESIAN_POINT ( 'NONE',  ( -20.29730442459490547, 222.0357903062123341, -14.50085278415678403 ) ) ;
#6174 = CARTESIAN_POINT ( 'NONE',  ( -35.09675569278795848, 415.7448905683720000, 15.47720386886985366 ) ) ;
#6175 = VECTOR ( 'NONE', #2870, 1000.000000000000000 ) ;
#6176 = CARTESIAN_POINT ( 'NONE',  ( -40.01497788969913216, 320.4323905765655809, -16.95518130045146421 ) ) ;
#6177 = DIRECTION ( 'NONE',  ( 0.000000000000000000, -1.000000000000000000, 0.000000000000000000 ) ) ;
#6178 = CARTESIAN_POINT ( 'NONE',  ( -11.93348319268871194, 288.5573905683720000, 3.332260488124728859 ) ) ;
#6179 = CARTESIAN_POINT ( 'NONE',  ( -44.16309181155858710, 464.7448905683720568, -6.410867750099231266 ) ) ;
#6180 = EDGE_CURVE ( 'NONE', #13749, #14150, #8739, .T. ) ;
#6181 = CARTESIAN_POINT ( 'NONE',  ( -40.01497788969914637, 458.8073905601784759, 16.95518130045146776 ) ) ;
#6182 = CARTESIAN_POINT ( 'NONE',  ( -64.27068722059111394, 600.7448905601785327, 35.12437985717896538 ) ) ;
#6183 = CARTESIAN_POINT ( 'NONE',  ( -49.57497958038186425, 230.5765313837437418, -49.99999999999999289 ) ) ;
#6184 = CARTESIAN_POINT ( 'NONE',  ( -40.53162694259543741, 374.1198905683720000, -11.84573899990672707 ) ) ;
#6185 = CARTESIAN_POINT ( 'NONE',  ( -16.84014894278200458, 507.6198905683720000, 11.84573899990672530 ) ) ;
#6186 = CARTESIAN_POINT ( 'NONE',  ( -48.68588794268872277, 506.9323905601784759, -3.978247347593158345 ) ) ;
#6187 = CARTESIAN_POINT ( 'NONE',  ( -22.27502019258948351, 320.7448905683720000, -15.47720386886985544 ) ) ;
#6188 = VECTOR ( 'NONE', #10482, 1000.000000000000000 ) ;
#6189 = VERTEX_POINT ( 'NONE', #20246 ) ;
#6190 = CARTESIAN_POINT ( 'NONE',  ( -8.685887942688740537, 522.2448905601784190, -2.449293598294705724E-15 ) ) ;
#6191 = ORIENTED_EDGE ( 'NONE', *, *, #14386, .F. ) ;
#6192 = LINE ( 'NONE', #16164, #5652 ) ;
#6193 = CARTESIAN_POINT ( 'NONE',  ( -14.48388495494900674, 429.4323905683720000, 9.489475012073731008 ) ) ;
#6194 = CARTESIAN_POINT ( 'NONE',  ( -48.68588794268887909, 392.3073905765655240, 3.978247347592742678 ) ) ;
#6195 = FACE_OUTER_BOUND ( 'NONE', #13821, .T. ) ;
#6196 = CARTESIAN_POINT ( 'NONE',  ( -45.43829269268871940, 453.5573905683720568, -3.332260488124726194 ) ) ;
#6197 = VERTEX_POINT ( 'NONE', #6830 ) ;
#6198 = CARTESIAN_POINT ( 'NONE',  ( -42.88789093042844769, 472.9323905683720568, -9.489475012073734561 ) ) ;
#6199 = DIRECTION ( 'NONE',  ( 0.000000000000000000, -1.000000000000000000, 0.000000000000000000 ) ) ;
#6200 = LINE ( 'NONE', #10961, #11368 ) ;
#6201 = CARTESIAN_POINT ( 'NONE',  ( -40.01497788969913216, 383.5573905765655809, 16.95518130045146776 ) ) ;
#6202 = CARTESIAN_POINT ( 'NONE',  ( 6.416697501590670427, 172.9933428177121471, 45.00000000000000000 ) ) ;
#6203 = DIRECTION ( 'NONE',  ( -1.191790137725560488E-16, 1.000000000000000000, 0.000000000000000000 ) ) ;
#6204 = PLANE ( 'NONE',  #20169 ) ;
#6205 = CARTESIAN_POINT ( 'NONE',  ( 60.74769842942832554, 56.85652257517428865, 40.00000000000000000 ) ) ;
#6206 = CARTESIAN_POINT ( 'NONE',  ( 171.3141120573112630, 610.7448905601785327, 0.000000000000000000 ) ) ;
#6207 = CARTESIAN_POINT ( 'NONE',  ( 4.700000000000000178, -3.752776749732576356, -6.499999999999999112 ) ) ;
#6208 = DIRECTION ( 'NONE',  ( 0.9864615503757148129, 0.000000000000000000, -0.1639927121256943288 ) ) ;
#6209 = CARTESIAN_POINT ( 'NONE',  ( -11.93348319268872970, 430.6823905683720568, -3.332260488124732856 ) ) ;
#6210 = CARTESIAN_POINT ( 'NONE',  ( -40.01497788969913927, 385.6823905601784190, -16.95518130045146421 ) ) ;
#6211 = CARTESIAN_POINT ( 'NONE',  ( -13.20868407381884779, 240.9948905683720284, -6.410867750099233042 ) ) ;
#6212 = ORIENTED_EDGE ( 'NONE', *, *, #16648, .T. ) ;
#6213 = VERTEX_POINT ( 'NONE', #11602 ) ;
#6214 = CARTESIAN_POINT ( 'NONE',  ( -41.83569717483972994, 230.5765313837437418, 25.00000000000000000 ) ) ;
#6215 = ORIENTED_EDGE ( 'NONE', *, *, #3113, .T. ) ;
#6216 = CARTESIAN_POINT ( 'NONE',  ( -45.43829269268872650, 465.0573905683720568, -3.332260488124726638 ) ) ;
#6217 = CARTESIAN_POINT ( 'NONE',  ( -42.82802356641964536, 223.2448905765656093, 14.14213562373094923 ) ) ;
#6218 = ADVANCED_FACE ( 'NONE', ( #6727 ), #14864, .F. ) ;
#6219 = VECTOR ( 'NONE', #8574, 1000.000000000000000 ) ;
#6220 = VERTEX_POINT ( 'NONE', #20037 ) ;
#6221 = FACE_OUTER_BOUND ( 'NONE', #19635, .T. ) ;
#6222 = CARTESIAN_POINT ( 'NONE',  ( -32.01814843081346851, 533.1823905683720568, -16.75240474999999307 ) ) ;
#6223 = VERTEX_POINT ( 'NONE', #11707 ) ;
#6224 = CARTESIAN_POINT ( 'NONE',  ( -14.48388495494901740, 527.9323905683720568, 9.489475012073731008 ) ) ;
#6225 = CARTESIAN_POINT ( 'NONE',  ( -28.68588794268872633, 230.8848358243226073, 0.000000000000000000 ) ) ;
#6226 = VECTOR ( 'NONE', #2436, 1000.000000000000000 ) ;
#6227 = CARTESIAN_POINT ( 'NONE',  ( -36.33955658999052218, 433.8698905765655809, 18.47759065022572500 ) ) ;
#6228 = CARTESIAN_POINT ( 'NONE',  ( -21.03221929538690915, 350.3698905601784759, 18.47759065022572500 ) ) ;
#6229 = EDGE_CURVE ( 'NONE', #2535, #7734, #1777, .T. ) ;
#6230 = CARTESIAN_POINT ( 'NONE',  ( 51.50493485826542184, 170.1716627696692683, 20.00000000000000355 ) ) ;
#6231 = CARTESIAN_POINT ( 'NONE',  ( -13.68588794268874054, 573.2448905601785327, 1.836970198721029589E-15 ) ) ;
#6232 = PLANE ( 'NONE',  #5656 ) ;
#6233 = CARTESIAN_POINT ( 'NONE',  ( -8.685887942688726326, 406.9948905765656377, -2.449293598294705724E-15 ) ) ;
#6234 = PLANE ( 'NONE',  #7631 ) ;
#6235 = AXIS2_PLACEMENT_3D ( 'NONE', #19220, #2572, #14152 ) ;
#6236 = CARTESIAN_POINT ( 'NONE',  ( -28.68588794268871212, 322.8698905683720000, -16.75240474999999307 ) ) ;
#6237 = CARTESIAN_POINT ( 'NONE',  ( 5.674999999999999822, 3.752776749732562589, 6.500000000000000000 ) ) ;
#6238 = FACE_OUTER_BOUND ( 'NONE', #504, .T. ) ;
#6239 = CARTESIAN_POINT ( 'NONE',  ( -28.68588794268873698, 56.85652257517428865, 0.000000000000000000 ) ) ;
#6240 = CARTESIAN_POINT ( 'NONE',  ( -25.35362745456398414, 302.5573905683720000, -16.75240474999999307 ) ) ;
#6241 = CIRCLE ( 'NONE', #6592, 175.0000000000000284 ) ;
#6242 = CARTESIAN_POINT ( 'NONE',  ( -40.53162694259543741, 355.1198905683720568, 11.84573899990672885 ) ) ;
#6243 = AXIS2_PLACEMENT_3D ( 'NONE', #11238, #19465, #4545 ) ;
#6244 = CARTESIAN_POINT ( 'NONE',  ( -22.27502019258949417, 518.4948905683719431, 15.47720386886985189 ) ) ;
#6245 = CARTESIAN_POINT ( 'NONE',  ( -42.82802356641965957, 375.9948905601784759, -14.14213562373094746 ) ) ;
#6246 = EDGE_CURVE ( 'NONE', #11848, #15984, #20766, .T. ) ;
#6247 = CARTESIAN_POINT ( 'NONE',  ( 5.074999999999999289, 6.500000000000000888, 0.000000000000000000 ) ) ;
#6248 = ORIENTED_EDGE ( 'NONE', *, *, #12533, .T. ) ;
#6249 = CARTESIAN_POINT ( 'NONE',  ( -28.68588794268872988, 482.8698905683720568, -16.75240474999999307 ) ) ;
#6250 = CARTESIAN_POINT ( 'NONE',  ( 88.15330054274429017, 79.55187051032177692, 94.99999999999994316 ) ) ;
#6251 = CARTESIAN_POINT ( 'NONE',  ( -16.84014894278198327, 290.1198905683720568, -11.84573899990672707 ) ) ;
#6252 = ORIENTED_EDGE ( 'NONE', *, *, #16463, .F. ) ;
#6253 = CARTESIAN_POINT ( 'NONE',  ( -25.35362745456398059, 282.5573905683720568, -16.75240474999999307 ) ) ;
#6254 = CARTESIAN_POINT ( 'NONE',  ( -25.35362745456397704, 316.6823905683720000, 16.75240474999998952 ) ) ;
#6255 = CARTESIAN_POINT ( 'NONE',  ( -35.09675569278793006, 263.4948905683720000, -15.47720386886985544 ) ) ;
#6256 = CARTESIAN_POINT ( 'NONE',  ( -14.54375231895775400, 255.7448905765656377, 14.14213562373094568 ) ) ;
#6257 = CARTESIAN_POINT ( 'NONE',  ( -47.16347859291445843, 476.6198905601785327, -7.653668647301793193 ) ) ;
#6258 = CARTESIAN_POINT ( 'NONE',  ( -11.93348319268870483, 228.8698905683720284, -2.051577885510841163E-15 ) ) ;
#6259 = CARTESIAN_POINT ( 'NONE',  ( -32.01814843081344719, 383.1823905683720568, -16.75240474999999307 ) ) ;
#6260 = EDGE_CURVE ( 'NONE', #3963, #9090, #4116, .T. ) ;
#6261 = CARTESIAN_POINT ( 'NONE',  ( -43.15146482487497792, 202.0901544311013538, 3.972812079771462113 ) ) ;
#6262 = CARTESIAN_POINT ( 'NONE',  ( 0.000000000000000000, -5.629165124598848990, -3.250000000000004441 ) ) ;
#6263 = CYLINDRICAL_SURFACE ( 'NONE', #479, 6.500000000000000888 ) ;
#6264 = CARTESIAN_POINT ( 'NONE',  ( -22.27502019258949773, 450.7448905683720000, -15.47720386886985544 ) ) ;
#6265 = FACE_OUTER_BOUND ( 'NONE', #7356, .T. ) ;
#6266 = ORIENTED_EDGE ( 'NONE', *, *, #6387, .T. ) ;
#6267 = CARTESIAN_POINT ( 'NONE',  ( -45.64106924314019409, 426.3073905601785327, -11.32908994701042715 ) ) ;
#6268 = EDGE_CURVE ( 'NONE', #2721, #15709, #7247, .T. ) ;
#6269 = EDGE_LOOP ( 'NONE', ( #18718, #15425, #20276, #15241 ) ) ;
#6270 = ORIENTED_EDGE ( 'NONE', *, *, #14849, .F. ) ;
#6271 = CARTESIAN_POINT ( 'NONE',  ( -28.68588794268873698, 548.2448905601784190, 0.000000000000000000 ) ) ;
#6272 = AXIS2_PLACEMENT_3D ( 'NONE', #20015, #7225, #16881 ) ;
#6273 = CARTESIAN_POINT ( 'NONE',  ( -28.68588794268870856, 319.7448905601785327, 19.99999999999999289 ) ) ;
#6274 = CARTESIAN_POINT ( 'NONE',  ( -28.68588794268869790, 223.9102039777116602, 0.000000000000000000 ) ) ;
#6275 = AXIS2_PLACEMENT_3D ( 'NONE', #9796, #14378, #16205 ) ;
#6276 = CARTESIAN_POINT ( 'NONE',  ( -13.20868407381885845, 350.9948905683720000, -6.410867750099233042 ) ) ;
#6277 = CARTESIAN_POINT ( 'NONE',  ( -48.68588794268872988, 511.6823905765655809, -3.978247347593158345 ) ) ;
#6278 = CARTESIAN_POINT ( 'NONE',  ( -28.68588794268871922, 391.3698905683720000, -16.75240474999999307 ) ) ;
#6279 = CARTESIAN_POINT ( 'NONE',  ( -25.35362745456396283, 228.1823905683720284, 16.75240474999998952 ) ) ;
#6280 = CARTESIAN_POINT ( 'NONE',  ( -22.27502019258947996, 376.9948905683720568, 15.47720386886985189 ) ) ;
#6281 = CARTESIAN_POINT ( 'NONE',  ( -11.73070664223724613, 317.9323905765656377, -11.32908994701042715 ) ) ;
#6282 = DIRECTION ( 'NONE',  ( 0.000000000000000000, -1.000000000000000000, 0.000000000000000000 ) ) ;
#6283 = CARTESIAN_POINT ( 'NONE',  ( -45.43829269268870519, 293.8698905683720568, 0.000000000000000000 ) ) ;
#6284 =( NAMED_UNIT ( * ) PLANE_ANGLE_UNIT ( ) SI_UNIT ( $, .RADIAN. ) );
#6285 = CARTESIAN_POINT ( 'NONE',  ( -32.01814843081345430, 447.5573905683720000, 16.75240474999999307 ) ) ;
#6286 = CARTESIAN_POINT ( 'NONE',  ( 20.74841189052421697, 600.7448905601785327, -7.500000000000000000 ) ) ;
#6287 = CARTESIAN_POINT ( 'NONE',  ( -3.933621007048970775E-15, 5.788408252967900403, 2.974182810908597485 ) ) ;
#6288 = DIRECTION ( 'NONE',  ( 0.000000000000000000, 0.000000000000000000, -1.000000000000000000 ) ) ;
#6289 = VECTOR ( 'NONE', #14093, 1000.000000000000000 ) ;
#6290 = CARTESIAN_POINT ( 'NONE',  ( -35.09675569278795138, 347.2448905683720000, 15.47720386886985366 ) ) ;
#6291 = CARTESIAN_POINT ( 'NONE',  ( -42.88789093042844769, 502.9323905683720000, -9.489475012073736337 ) ) ;
#6292 = CARTESIAN_POINT ( 'NONE',  ( -14.54375231895778242, 490.9948905601784759, 14.14213562373094568 ) ) ;
#6293 = CARTESIAN_POINT ( 'NONE',  ( -42.88789093042843348, 332.9323905683720568, -9.489475012073736337 ) ) ;
#6294 = ORIENTED_EDGE ( 'NONE', *, *, #14622, .T. ) ;
#6295 = CARTESIAN_POINT ( 'NONE',  ( 91.21585410611801592, 31.85652257517428865, -85.46735025547123143 ) ) ;
#6296 = PRODUCT_DEFINITION_SHAPE ( 'NONE', 'NONE',  #18472 ) ;
#6297 = ORIENTED_EDGE ( 'NONE', *, *, #12814, .F. ) ;
#6298 = CARTESIAN_POINT ( 'NONE',  ( -32.25189173780753293, 50.98147789719760681, 49.47307091579321536 ) ) ;
#6299 = EDGE_CURVE ( 'NONE', #17635, #18850, #13875, .T. ) ;
#6300 = AXIS2_PLACEMENT_3D ( 'NONE', #15753, #20829, #5890 ) ;
#6301 = EDGE_CURVE ( 'NONE', #74, #4920, #5634, .T. ) ;
#6302 = CARTESIAN_POINT ( 'NONE',  ( -25.35362745456398770, 408.1823905683720000, 16.75240474999998952 ) ) ;
#6303 = CARTESIAN_POINT ( 'NONE',  ( -48.68588794268870146, 291.9948905765656377, 0.000000000000000000 ) ) ;
#6304 = CARTESIAN_POINT ( 'NONE',  ( -42.88789093042844769, 452.9323905683720568, -9.489475012073736337 ) ) ;
#6305 = ORIENTED_EDGE ( 'NONE', *, *, #14782, .F. ) ;
#6306 = CARTESIAN_POINT ( 'NONE',  ( -45.43829269268872650, 453.5573905683720568, -3.332260488124726638 ) ) ;
#6307 = DIRECTION ( 'NONE',  ( 0.000000000000000000, 0.000000000000000000, -1.000000000000000000 ) ) ;
#6308 = CARTESIAN_POINT ( 'NONE',  ( -71.26501780185373036, 205.1437886375728965, -5.000000000000001776 ) ) ;
#6309 = CARTESIAN_POINT ( 'NONE',  ( -10.20829729246298889, 386.3698905765656377, 7.653668647301790529 ) ) ;
#6310 = CARTESIAN_POINT ( 'NONE',  ( -31.26501780185373391, 205.1437886375728965, 0.000000000000000000 ) ) ;
#6311 = CARTESIAN_POINT ( 'NONE',  ( -47.16347859291444422, 371.3698905765655809, -7.653668647301793193 ) ) ;
#6312 = CARTESIAN_POINT ( 'NONE',  ( -14.54375231895777887, 428.2448905765656377, -14.14213562373094746 ) ) ;
#6313 = DIRECTION ( 'NONE',  ( 0.000000000000000000, -0.000000000000000000, -1.000000000000000000 ) ) ;
#6314 = CARTESIAN_POINT ( 'NONE',  ( -25.35362745456400901, 502.5573905683719431, -16.75240474999999307 ) ) ;
#6315 = DIRECTION ( 'NONE',  ( -0.000000000000000000, 0.000000000000000000, 1.000000000000000000 ) ) ;
#6316 = DIRECTION ( 'NONE',  ( -0.000000000000000000, -1.000000000000000000, -0.000000000000000000 ) ) ;
#6317 = CARTESIAN_POINT ( 'NONE',  ( 158.8141120573112630, 610.7448905601785327, 0.000000000000000000 ) ) ;
#6318 = AXIS2_PLACEMENT_3D ( 'NONE', #14048, #14375, #10884 ) ;
#6319 = CARTESIAN_POINT ( 'NONE',  ( -11.93348319268872615, 410.3698905683720568, -2.051577885510841163E-15 ) ) ;
#6320 = CARTESIAN_POINT ( 'NONE',  ( -21.03221929538690205, 265.1198905765655809, 18.47759065022572500 ) ) ;
#6321 = CARTESIAN_POINT ( 'NONE',  ( -40.53162694259542320, 244.1198905683720284, -11.84573899990672707 ) ) ;
#6322 = ORIENTED_EDGE ( 'NONE', *, *, #11218, .T. ) ;
#6323 = ORIENTED_EDGE ( 'NONE', *, *, #16235, .F. ) ;
#6324 = DIRECTION ( 'NONE',  ( -1.191790137725560488E-16, 1.000000000000000000, -0.000000000000000000 ) ) ;
#6325 = VERTEX_POINT ( 'NONE', #2402 ) ;
#6326 = CARTESIAN_POINT ( 'NONE',  ( -11.93348319268873503, 470.3698905683720568, -2.051577885510841163E-15 ) ) ;
#6327 = CARTESIAN_POINT ( 'NONE',  ( -11.73070664223723014, 226.0573905765655809, 11.32908994701042005 ) ) ;
#6328 = AXIS2_PLACEMENT_3D ( 'NONE', #6351, #7546, #14171 ) ;
#6329 = ORIENTED_EDGE ( 'NONE', *, *, #9299, .T. ) ;
#6330 = CARTESIAN_POINT ( 'NONE',  ( -8.685887942688729879, 432.2448905601785327, -2.449293598294705724E-15 ) ) ;
#6331 = CARTESIAN_POINT ( 'NONE',  ( -19.19641293061497223, 230.4323905683720000, -14.20200298773971603 ) ) ;
#6332 = VECTOR ( 'NONE', #20828, 1000.000000000000000 ) ;
#6333 = ORIENTED_EDGE ( 'NONE', *, *, #3620, .T. ) ;
#6334 = CARTESIAN_POINT ( 'NONE',  ( -22.27502019258950483, 530.7448905683720568, -15.47720386886985544 ) ) ;
#6335 = DIRECTION ( 'NONE',  ( 2.399110633850889130E-16, 0.000000000000000000, -1.000000000000000000 ) ) ;
#6336 = CARTESIAN_POINT ( 'NONE',  ( -21.03221929538693402, 448.8698905765656377, -18.47759065022572855 ) ) ;
#6337 = CARTESIAN_POINT ( 'NONE',  ( -13.20868407381885667, 338.2448905683720568, 6.410867750099229490 ) ) ;
#6338 = CARTESIAN_POINT ( 'NONE',  ( -47.16347859291445843, 452.6198905765656377, 7.653668647301805628 ) ) ;
#6339 = CARTESIAN_POINT ( 'NONE',  ( -14.54375231895775578, 238.2448905765656093, -14.14213562373094746 ) ) ;
#6340 = CARTESIAN_POINT ( 'NONE',  ( -36.33955658999050797, 289.1198905601785327, 18.47759065022572500 ) ) ;
#6341 = FACE_OUTER_BOUND ( 'NONE', #20011, .T. ) ;
#6342 = CARTESIAN_POINT ( 'NONE',  ( 27.98965548446208373, 333.8848358243226357, 40.00000000000000000 ) ) ;
#6343 = CARTESIAN_POINT ( 'NONE',  ( -22.27502019258948351, 322.2448905683720000, -15.47720386886985544 ) ) ;
#6344 = CARTESIAN_POINT ( 'NONE',  ( -8.685887942688742314, 532.2448905601784190, -2.449293598294705724E-15 ) ) ;
#6345 = CARTESIAN_POINT ( 'NONE',  ( 65.85920792673738333, 160.1716627696692683, 20.00000000000000355 ) ) ;
#6346 = VECTOR ( 'NONE', #6766, 1000.000000000000000 ) ;
#6347 = CARTESIAN_POINT ( 'NONE',  ( -16.84014894278197971, 309.1198905683720000, 11.84573899990672530 ) ) ;
#6348 = EDGE_CURVE ( 'NONE', #5058, #15419, #8984, .T. ) ;
#6349 = CARTESIAN_POINT ( 'NONE',  ( -45.43829269268873361, 515.3698905683720568, 0.000000000000000000 ) ) ;
#6350 = CARTESIAN_POINT ( 'NONE',  ( -45.64106924314018698, 376.3073905601784759, -11.32908994701042715 ) ) ;
#6351 = CARTESIAN_POINT ( 'NONE',  ( 43.53705524234220547, -133.1434774248255906, -96.62835994548002816 ) ) ;
#6352 = VERTEX_POINT ( 'NONE', #9091 ) ;
#6353 = CARTESIAN_POINT ( 'NONE',  ( -44.16309181155858710, 484.7448905683720568, -6.410867750099231266 ) ) ;
#6354 = CARTESIAN_POINT ( 'NONE',  ( 51.98438129372387806, 56.85652257517428865, 117.7249735956185219 ) ) ;
#6355 = CARTESIAN_POINT ( 'NONE',  ( -28.68588794268870146, 276.3698905683720000, 16.75240474999999307 ) ) ;
#6356 = VERTEX_POINT ( 'NONE', #15710 ) ;
#6357 = CARTESIAN_POINT ( 'NONE',  ( -11.93348319268871016, 280.3698905683720000, -2.051577885510841163E-15 ) ) ;
#6358 = CARTESIAN_POINT ( 'NONE',  ( -38.17536295476244135, 325.4323905683720000, 14.20200298773971781 ) ) ;
#6359 = CARTESIAN_POINT ( 'NONE',  ( -38.17536295476243424, 256.9323905683720000, 14.20200298773971781 ) ) ;
#6360 = CARTESIAN_POINT ( 'NONE',  ( -48.68588794268869435, 261.9948905765655809, 0.000000000000000000 ) ) ;
#6361 = CARTESIAN_POINT ( 'NONE',  ( -10.20829729246299955, 472.8698905601784759, -7.653668647301794969 ) ) ;
#6362 = CARTESIAN_POINT ( 'NONE',  ( -42.88789093042841927, 224.8073905683720000, 9.489475012073734561 ) ) ;
#6363 = CARTESIAN_POINT ( 'NONE',  ( -22.27502019258947641, 368.4948905683720568, 15.47720386886985189 ) ) ;
#6364 = EDGE_CURVE ( 'NONE', #8749, #18802, #896, .T. ) ;
#6365 = CARTESIAN_POINT ( 'NONE',  ( -28.68588794268874054, 588.2448905601785327, 0.000000000000000000 ) ) ;
#6366 = CARTESIAN_POINT ( 'NONE',  ( -8.685887942688710339, 262.2448905601784759, -2.449293598294705724E-15 ) ) ;
#6367 = FACE_OUTER_BOUND ( 'NONE', #14070, .T. ) ;
#6368 = CARTESIAN_POINT ( 'NONE',  ( -40.53162694259544452, 422.6198905683720000, -11.84573899990672707 ) ) ;
#6369 = DIRECTION ( 'NONE',  ( -1.000000000000000000, -0.000000000000000000, -0.000000000000000000 ) ) ;
#6370 = EDGE_LOOP ( 'NONE', ( #1038, #426 ) ) ;
#6371 = CARTESIAN_POINT ( 'NONE',  ( -28.68588794268872277, 424.7448905601784759, -19.99999999999999289 ) ) ;
#6372 = ORIENTED_EDGE ( 'NONE', *, *, #9426, .T. ) ;
#6373 = VERTEX_POINT ( 'NONE', #20671 ) ;
#6374 = ORIENTED_EDGE ( 'NONE', *, *, #388, .F. ) ;
#6375 = CARTESIAN_POINT ( 'NONE',  ( -43.63240530816146645, 209.9813655751484305, -1.306613905557860500 ) ) ;
#6376 = CARTESIAN_POINT ( 'NONE',  ( -40.01497788969912506, 308.8073905601784759, 16.95518130045146776 ) ) ;
#6377 = CARTESIAN_POINT ( 'NONE',  ( -28.68588794268872633, 378.8848358243226357, -20.00000000000000000 ) ) ;
#6378 = EDGE_CURVE ( 'NONE', #7175, #10958, #14293, .T. ) ;
#6379 = CARTESIAN_POINT ( 'NONE',  ( -28.68588794268870856, 337.8698905683720000, 16.75240474999999307 ) ) ;
#6380 = CARTESIAN_POINT ( 'NONE',  ( -21.03221929538694113, 508.8698905765656377, -18.47759065022572855 ) ) ;
#6381 = CARTESIAN_POINT ( 'NONE',  ( -44.16309181155857999, 393.2448905683720568, -6.410867750099231266 ) ) ;
#6382 = CARTESIAN_POINT ( 'NONE',  ( -45.43829269268869098, 225.0573905683720568, -3.332260488124726194 ) ) ;
#6383 = CARTESIAN_POINT ( 'NONE',  ( -13.20868407381886200, 388.2448905683720000, 6.410867750099229490 ) ) ;
#6384 = CARTESIAN_POINT ( 'NONE',  ( -14.54375231895776643, 328.2448905765656377, -14.14213562373094746 ) ) ;
#6385 = CARTESIAN_POINT ( 'NONE',  ( -48.68588794268871567, 427.2448905601784759, 0.000000000000000000 ) ) ;
#6386 = CARTESIAN_POINT ( 'NONE',  ( -11.93348319268871016, 278.5573905683720568, 3.332260488124728859 ) ) ;
#6387 = EDGE_CURVE ( 'NONE', #12984, #21078, #19920, .T. ) ;
#6388 = CARTESIAN_POINT ( 'NONE',  ( -45.43829269268871229, 445.6823905683720000, 3.332260488124734632 ) ) ;
#6389 = ADVANCED_FACE ( 'NONE', ( #19680 ), #6906, .F. ) ;
#6390 = CARTESIAN_POINT ( 'NONE',  ( -36.33955658999050087, 285.3698905601784759, -18.47759065022572855 ) ) ;
#6391 = CARTESIAN_POINT ( 'NONE',  ( 20.42502041961813930, 230.5765313837437418, -60.00000000000000000 ) ) ;
#6392 = LINE ( 'NONE', #1543, #2997 ) ;
#6393 = CARTESIAN_POINT ( 'NONE',  ( -35.09675569278794427, 353.4948905683720000, -15.47720386886985544 ) ) ;
#6394 = CARTESIAN_POINT ( 'NONE',  ( -45.43829269268871940, 473.5573905683720000, -3.332260488124726194 ) ) ;
#6395 = CARTESIAN_POINT ( 'NONE',  ( -48.68588794268872277, 477.2448905601784759, 0.000000000000000000 ) ) ;
#6396 = CARTESIAN_POINT ( 'NONE',  ( -14.48388495494899608, 329.8073905683720000, -9.489475012073736337 ) ) ;
#6397 = ORIENTED_EDGE ( 'NONE', *, *, #21057, .T. ) ;
#6398 = CARTESIAN_POINT ( 'NONE',  ( 60.03793209889851568, 30.52886280891152282, 131.1729372809869005 ) ) ;
#6399 = VERTEX_POINT ( 'NONE', #16452 ) ;
#6400 = LINE ( 'NONE', #11379, #19840 ) ;
#6401 =( BOUNDED_CURVE ( )  B_SPLINE_CURVE ( 2, ( #8683, #6848, #4030, #3817, #18628, #20369, #16818, #20166, #5332, #5437, #13464, #15410, #3613, #16924, #11933, #8576, #11831 ),
 .UNSPECIFIED., .F., .T. ) 
 B_SPLINE_CURVE_WITH_KNOTS ( ( 3, 2, 2, 2, 2, 2, 2, 2, 3 ),
 ( 0.2968750000000001110, 0.2988281250000001110, 0.3007812500000001110, 0.3027343750000001110, 0.3046875000000001110, 0.3066406250000001110, 0.3085937500000001110, 0.3105468750000001110, 0.3125000000000001110 ),
 .UNSPECIFIED. ) 
 CURVE ( )  GEOMETRIC_REPRESENTATION_ITEM ( )  RATIONAL_B_SPLINE_CURVE ( ( 0.9999999999999988898, 0.9807852804032315408, 1.000000000000000000, 0.9807852804032304306, 1.000000000000000000, 0.9807852804032304306, 1.000000000000000000, 0.9807852804032304306, 1.000000000000000000, 0.9807852804032304306, 1.000000000000000000, 0.9807852804032304306, 1.000000000000000000, 0.9807852804032304306, 1.000000000000000000, 0.9807852804032293204, 1.000000000000001110 ) ) 
 REPRESENTATION_ITEM ( '' )  );
#6402 = CARTESIAN_POINT ( 'NONE',  ( -42.88789093042844058, 406.3073905683719431, 9.489475012073734561 ) ) ;
#6403 = CARTESIAN_POINT ( 'NONE',  ( -32.66413529028187668, 394.1823905765655809, 19.99999999999999289 ) ) ;
#6404 = DIRECTION ( 'NONE',  ( -0.000000000000000000, 1.000000000000000000, -0.000000000000000000 ) ) ;
#6405 = CARTESIAN_POINT ( 'NONE',  ( -16.84014894278200103, 440.1198905683720568, -11.84573899990672707 ) ) ;
#6406 = CARTESIAN_POINT ( 'NONE',  ( -45.43829269268871940, 443.8698905683720568, 0.000000000000000000 ) ) ;
#6407 = CARTESIAN_POINT ( 'NONE',  ( -48.68588794268873698, 573.2448905601785327, 0.000000000000000000 ) ) ;
#6408 = CARTESIAN_POINT ( 'NONE',  ( -10.20829729246298889, 387.6198905765655809, -7.653668647301794969 ) ) ;
#6409 = CARTESIAN_POINT ( 'NONE',  ( -13.59795901728759482, 49.21534327078636295, 47.25690868943056699 ) ) ;
#6410 = CARTESIAN_POINT ( 'NONE',  ( -11.73070664223725323, 387.9323905765656377, -11.32908994701042538 ) ) ;
#6411 = FACE_OUTER_BOUND ( 'NONE', #7242, .T. ) ;
#6412 = PLANE ( 'NONE',  #4579 ) ;
#6413 = CARTESIAN_POINT ( 'NONE',  ( -40.53162694259545162, 504.1198905683720568, -11.84573899990672707 ) ) ;
#6414 = CARTESIAN_POINT ( 'NONE',  ( 115.7989814974898195, 160.1716627696691830, 20.00000000000000355 ) ) ;
#6415 = CARTESIAN_POINT ( 'NONE',  ( -45.64106924314018698, 418.1823905601784759, 11.32908994701042538 ) ) ;
#6416 = CIRCLE ( 'NONE', #7467, 20.00000000000000000 ) ;
#6417 = CARTESIAN_POINT ( 'NONE',  ( -42.88789093042844058, 416.3073905683720568, 9.489475012073736337 ) ) ;
#6418 = CARTESIAN_POINT ( 'NONE',  ( -28.68588794268871922, 384.7448905601785327, -19.99999999999999289 ) ) ;
#6419 = CARTESIAN_POINT ( 'NONE',  ( -25.35362745456396283, 228.1823905683720284, 16.75240474999998952 ) ) ;
#6420 = CIRCLE ( 'NONE', #19915, 5.000000000000004441 ) ;
#6421 = ORIENTED_EDGE ( 'NONE', *, *, #4665, .T. ) ;
#6422 = CARTESIAN_POINT ( 'NONE',  ( -14.54375231895777532, 425.7448905765656377, 14.14213562373094568 ) ) ;
#6423 = EDGE_LOOP ( 'NONE', ( #14122, #10495 ) ) ;
#6424 = CARTESIAN_POINT ( 'NONE',  ( -42.88789093042844769, 454.4323905683720568, -9.489475012073734561 ) ) ;
#6425 = CARTESIAN_POINT ( 'NONE',  ( -17.35679799567827430, 225.4323905765655809, 16.95518130045146421 ) ) ;
#6426 = EDGE_CURVE ( 'NONE', #14255, #15845, #13529, .T. ) ;
#6427 = ORIENTED_EDGE ( 'NONE', *, *, #20063, .F. ) ;
#6428 = PLANE ( 'NONE',  #16609 ) ;
#6429 = CARTESIAN_POINT ( 'NONE',  ( -44.16309181155855157, 224.4948905683720284, 6.410867750099241924 ) ) ;
#6430 = EDGE_CURVE ( 'NONE', #6038, #16754, #8207, .T. ) ;
#6431 = EDGE_LOOP ( 'NONE', ( #4316, #2920, #6613, #11994 ) ) ;
#6432 = CARTESIAN_POINT ( 'NONE',  ( -44.16309181155857999, 504.4948905683720568, 6.410867750099241924 ) ) ;
#6433 = DIRECTION ( 'NONE',  ( -0.000000000000000000, -1.000000000000000000, -0.000000000000000000 ) ) ;
#6434 = EDGE_CURVE ( 'NONE', #16453, #10176, #5975, .T. ) ;
#6435 = CIRCLE ( 'NONE', #4728, 0.4000000000000001887 ) ;
#6436 = CARTESIAN_POINT ( 'NONE',  ( -42.82802356641967378, 453.2448905765656377, 14.14213562373094923 ) ) ;
#6437 = DIRECTION ( 'NONE',  ( -1.000000000000000000, 0.000000000000000000, 0.000000000000000000 ) ) ;
#6438 = CARTESIAN_POINT ( 'NONE',  ( -11.73070664223724258, 331.3073905601785327, 11.32908994701042005 ) ) ;
#6439 = CARTESIAN_POINT ( 'NONE',  ( 125.7989814974898053, 10.52886280891152104, 40.00000000000000000 ) ) ;
#6440 = DIRECTION ( 'NONE',  ( -1.000000000000000000, 0.000000000000000000, 0.000000000000000000 ) ) ;
#6441 = CARTESIAN_POINT ( 'NONE',  ( 91.21585410611801592, 31.85652257517428865, 40.00000000000000000 ) ) ;
#6442 = AXIS2_PLACEMENT_3D ( 'NONE', #14353, #6002, #17788 ) ;
#6443 = CARTESIAN_POINT ( 'NONE',  ( -40.53162694259542320, 222.6198905683720000, -11.84573899990672707 ) ) ;
#6444 = CARTESIAN_POINT ( 'NONE',  ( -25.35362745456398414, 312.5573905683720000, -16.75240474999999307 ) ) ;
#6445 = EDGE_CURVE ( 'NONE', #2121, #4920, #17049, .T. ) ;
#6446 = CARTESIAN_POINT ( 'NONE',  ( -17.35679799567830628, 443.8073905601784759, -16.95518130045146421 ) ) ;
#6447 = CARTESIAN_POINT ( 'NONE',  ( -42.82802356641964536, 268.4948905601784759, 14.14213562373094923 ) ) ;
#6448 = DIRECTION ( 'NONE',  ( 0.000000000000000000, 0.000000000000000000, 1.000000000000000000 ) ) ;
#6449 = CARTESIAN_POINT ( 'NONE',  ( -35.09675569278794427, 287.2448905683720000, 15.47720386886985366 ) ) ;
#6450 = VECTOR ( 'NONE', #8707, 1000.000000000000000 ) ;
#6451 = CARTESIAN_POINT ( 'NONE',  ( -25.35362745456401257, 522.5573905683720568, -16.75240474999999307 ) ) ;
#6452 = CARTESIAN_POINT ( 'NONE',  ( -28.68588794268871567, 374.7448905601785327, -19.99999999999999289 ) ) ;
#6453 = VECTOR ( 'NONE', #5624, 1000.000000000000000 ) ;
#6454 = CARTESIAN_POINT ( 'NONE',  ( -24.70764059509555111, 314.4323905601784190, -19.99999999999999289 ) ) ;
#6455 = VERTEX_POINT ( 'NONE', #5287 ) ;
#6456 = CARTESIAN_POINT ( 'NONE',  ( -40.53162694259545162, 486.6198905683720000, 11.84573899990672885 ) ) ;
#6457 = CARTESIAN_POINT ( 'NONE',  ( 158.8141120573112630, 575.7448905601785327, -10.00000000000000888 ) ) ;
#6458 = CARTESIAN_POINT ( 'NONE',  ( -40.53162694259543031, 285.1198905683720568, 11.84573899990672885 ) ) ;
#6459 = ORIENTED_EDGE ( 'NONE', *, *, #7452, .F. ) ;
#6460 = CARTESIAN_POINT ( 'NONE',  ( -38.17536295476244135, 276.9323905683720000, 14.20200298773971781 ) ) ;
#6461 = CARTESIAN_POINT ( 'NONE',  ( -25.35362745456398414, 311.0573905683720568, -16.75240474999999307 ) ) ;
#6462 = CARTESIAN_POINT ( 'NONE',  ( -11.93348319268870839, 260.0573905683720000, 3.332260488124728859 ) ) ;
#6463 = VECTOR ( 'NONE', #6465, 1000.000000000000000 ) ;
#6464 = CARTESIAN_POINT ( 'NONE',  ( -36.33955658999049376, 260.1198905765655809, -18.47759065022572855 ) ) ;
#6465 = DIRECTION ( 'NONE',  ( -0.000000000000000000, -0.000000000000000000, -1.000000000000000000 ) ) ;
#6466 = CARTESIAN_POINT ( 'NONE',  ( -22.27502019258949062, 382.2448905683720000, -15.47720386886985544 ) ) ;
#6467 = CIRCLE ( 'NONE', #12006, 6.500000000000000888 ) ;
#6468 = CARTESIAN_POINT ( 'NONE',  ( 115.7989814974898337, 152.5259582928263740, -40.00000000000000000 ) ) ;
#6469 = PLANE ( 'NONE',  #15234 ) ;
#6470 = PRODUCT_DEFINITION_SHAPE ( 'NONE', 'NONE',  #21403 ) ;
#6471 = CARTESIAN_POINT ( 'NONE',  ( -32.66413529028185536, 269.8073905765655809, -19.99999999999999289 ) ) ;
#6472 = B_SPLINE_CURVE_WITH_KNOTS ( 'NONE', 3,
 ( #16134, #21099, #16243, #6375, #11247, #17845, #1419, #14837, #3255, #6480, #1317, #14, #19576, #4553, #4757, #6588, #11574, #7888 ),
 .UNSPECIFIED., .F., .F.,
 ( 4, 2, 2, 2, 2, 2, 2, 2, 4 ),
 ( 0.01574578602456870244, 0.01672957298347709995, 0.01771335994238549399, 0.01869714690129389151, 0.01968093386020228555, 0.02066472081911068306, 0.02164850777801907711, 0.02263229473692747462, 0.02361608169583586866 ),
 .UNSPECIFIED. ) ;
#6473 = CARTESIAN_POINT ( 'NONE',  ( -14.48388495494900674, 429.8073905683720000, -9.489475012073736337 ) ) ;
#6474 = PLANE ( 'NONE',  #13626 ) ;
#6475 = ORIENTED_EDGE ( 'NONE', *, *, #16308, .F. ) ;
#6476 = CARTESIAN_POINT ( 'NONE',  ( -24.70764059509556887, 434.4323905601784759, -19.99999999999999289 ) ) ;
#6477 = VERTEX_POINT ( 'NONE', #11890 ) ;
#6478 = EDGE_LOOP ( 'NONE', ( #4210, #16583, #17593, #7571, #14863, #1612, #6372, #1211, #6801, #8122, #10737, #7522, #19925, #14309, #20623 ) ) ;
#6479 = ORIENTED_EDGE ( 'NONE', *, *, #3225, .T. ) ;
#6480 = CARTESIAN_POINT ( 'NONE',  ( -43.20717515250593266, 208.4480206960199382, -3.766779594902115225 ) ) ;
#6481 = CARTESIAN_POINT ( 'NONE',  ( -24.70764059509555466, 304.4323905601784759, -19.99999999999999289 ) ) ;
#6482 = CARTESIAN_POINT ( 'NONE',  ( -42.88454851406326185, 206.4494888775581103, -4.837634058829628714 ) ) ;
#6483 = EDGE_CURVE ( 'NONE', #11897, #8381, #130, .T. ) ;
#6484 = CARTESIAN_POINT ( 'NONE',  ( -42.88789093042843348, 336.3073905683720568, 9.489475012073734561 ) ) ;
#6485 = CARTESIAN_POINT ( 'NONE',  ( -11.73070664223726389, 477.9323905765656377, -11.32908994701042715 ) ) ;
#6486 = CARTESIAN_POINT ( 'NONE',  ( -19.19641293061498644, 360.4323905683720000, -14.20200298773971603 ) ) ;
#6487 = CARTESIAN_POINT ( 'NONE',  ( -45.43829269268869808, 225.3698905683720284, 0.000000000000000000 ) ) ;
#6488 = CARTESIAN_POINT ( 'NONE',  ( -45.43829269268871229, 383.5573905683720000, -3.332260488124726638 ) ) ;
#6489 = CARTESIAN_POINT ( 'NONE',  ( -48.68588794268870146, 321.9948905765655809, 0.000000000000000000 ) ) ;
#6490 = LINE ( 'NONE', #4565, #19323 ) ;
#6491 = EDGE_CURVE ( 'NONE', #10771, #3667, #3643, .T. ) ;
#6492 = CARTESIAN_POINT ( 'NONE',  ( -16.84014894278197971, 280.1198905683720000, -11.84573899990672707 ) ) ;
#6493 = DIRECTION ( 'NONE',  ( 1.000000000000000000, 0.000000000000000000, 0.000000000000000000 ) ) ;
#6494 = CARTESIAN_POINT ( 'NONE',  ( -16.84014894278199748, 431.6198905683720000, -11.84573899990672707 ) ) ;
#6495 = CARTESIAN_POINT ( 'NONE',  ( 35.96497763894178945, 230.5765313837437418, 60.00000000000000000 ) ) ;
#6496 = CARTESIAN_POINT ( 'NONE',  ( -28.68588794268872988, 499.7448905601785327, 19.99999999999999289 ) ) ;
#6497 = LINE ( 'NONE', #14958, #11620 ) ;
#6498 = CARTESIAN_POINT ( 'NONE',  ( -8.685887942688731655, 452.2448905601784759, -2.449293598294705724E-15 ) ) ;
#6499 = CARTESIAN_POINT ( 'NONE',  ( -25.35362745456398770, 342.5573905683720568, -16.75240474999999307 ) ) ;
#6500 = CARTESIAN_POINT ( 'NONE',  ( -44.16309181155857999, 484.4948905683720000, 6.410867750099241924 ) ) ;
#6501 = EDGE_CURVE ( 'NONE', #7438, #10209, #10129, .T. ) ;
#6502 = EDGE_LOOP ( 'NONE', ( #12886, #5145, #1960, #7766, #6810, #17299, #15693 ) ) ;
#6503 = CARTESIAN_POINT ( 'NONE',  ( -45.64106924314020119, 486.3073905601785327, -11.32908994701042715 ) ) ;
#6504 = CARTESIAN_POINT ( 'NONE',  ( -40.53162694259543031, 302.6198905683720000, -11.84573899990672707 ) ) ;
#6505 = ORIENTED_EDGE ( 'NONE', *, *, #12118, .F. ) ;
#6506 = DIRECTION ( 'NONE',  ( 0.000000000000000000, 0.000000000000000000, -1.000000000000000000 ) ) ;
#6507 = ORIENTED_EDGE ( 'NONE', *, *, #6035, .T. ) ;
#6508 = CARTESIAN_POINT ( 'NONE',  ( -32.89591654994843140, 52.24166481711759502, 49.42222731526657498 ) ) ;
#6509 = AXIS2_PLACEMENT_3D ( 'NONE', #11041, #9428, #16046 ) ;
#6510 = ADVANCED_FACE ( 'NONE', ( #10468, #16985, #7011 ), #547, .F. ) ;
#6511 = CARTESIAN_POINT ( 'NONE',  ( -16.84014894278199037, 399.1198905683720000, 11.84573899990672530 ) ) ;
#6512 = DIRECTION ( 'NONE',  ( 0.4627175328665442677, 0.000000000000000000, -0.8865057725575724579 ) ) ;
#6513 = CARTESIAN_POINT ( 'NONE',  ( -28.68588794268872633, 174.3162933293988033, 0.000000000000000000 ) ) ;
#6514 = CARTESIAN_POINT ( 'NONE',  ( -11.93348319268872970, 438.8698905683720568, -2.051577885510841163E-15 ) ) ;
#6515 = CARTESIAN_POINT ( 'NONE',  ( -14.48388495494901029, 439.8073905683721136, -9.489475012073734561 ) ) ;
#6516 = CARTESIAN_POINT ( 'NONE',  ( -8.685887942688726326, 412.2448905601784759, -2.449293598294705724E-15 ) ) ;
#6517 = CARTESIAN_POINT ( 'NONE',  ( -17.35679799567829562, 385.4323905765655809, 16.95518130045146421 ) ) ;
#6518 = CARTESIAN_POINT ( 'NONE',  ( -28.68588794268874054, 573.2448905601785327, 0.000000000000000000 ) ) ;
#6519 = FACE_OUTER_BOUND ( 'NONE', #20785, .T. ) ;
#6520 = CARTESIAN_POINT ( 'NONE',  ( -8.685887942688628627, 487.3073905765656377, -3.978247347592898553 ) ) ;
#6521 = CARTESIAN_POINT ( 'NONE',  ( -45.43829269268871940, 505.6823905683720568, 3.332260488124734632 ) ) ;
#6522 = LINE ( 'NONE', #3507, #601 ) ;
#6523 = DIRECTION ( 'NONE',  ( -0.000000000000000000, 1.000000000000000000, -0.000000000000000000 ) ) ;
#6524 = CARTESIAN_POINT ( 'NONE',  ( -14.54375231895778597, 520.9948905601784190, 14.14213562373094568 ) ) ;
#6525 = VECTOR ( 'NONE', #14000, 1000.000000000000114 ) ;
#6526 = ADVANCED_FACE ( 'NONE', ( #10680 ), #7117, .T. ) ;
#6527 = CARTESIAN_POINT ( 'NONE',  ( -22.27502019258949062, 402.2448905683720568, -15.47720386886985544 ) ) ;
#6528 = CARTESIAN_POINT ( 'NONE',  ( -47.16347859291443001, 262.6198905765655809, 7.653668647301805628 ) ) ;
#6529 =( BOUNDED_CURVE ( )  B_SPLINE_CURVE ( 2, ( #18950, #1224, #15934, #4248, #17337, #20799, #2627, #12580, #2522, #7474, #14104, #14323, #5967, #20687, #2844, #19174, #5862 ),
 .UNSPECIFIED., .F., .T. ) 
 B_SPLINE_CURVE_WITH_KNOTS ( ( 3, 2, 2, 2, 2, 2, 2, 2, 3 ),
 ( 0.6562500000000000000, 0.6582031250000000000, 0.6601562500000000000, 0.6621093750000001110, 0.6640625000000001110, 0.6660156250000001110, 0.6679687500000002220, 0.6699218750000002220, 0.6718750000000002220 ),
 .UNSPECIFIED. ) 
 CURVE ( )  GEOMETRIC_REPRESENTATION_ITEM ( )  RATIONAL_B_SPLINE_CURVE ( ( 1.000000000000000000, 0.9807852804032304306, 1.000000000000000000, 0.9807852804032304306, 1.000000000000000000, 0.9807852804032304306, 1.000000000000000000, 0.9807852804032304306, 1.000000000000000000, 0.9807852804032304306, 1.000000000000000000, 0.9807852804032304306, 1.000000000000000000, 0.9807852804032304306, 1.000000000000000000, 0.9807852804032282101, 1.000000000000002220 ) ) 
 REPRESENTATION_ITEM ( '' )  );
#6530 = CARTESIAN_POINT ( 'NONE',  ( -14.48388495494898187, 229.4323905683720000, 9.489475012073732785 ) ) ;
#6531 = EDGE_LOOP ( 'NONE', ( #12619, #17533, #18014, #2397 ) ) ;
#6532 = CARTESIAN_POINT ( 'NONE',  ( 81.24038404635966515, 30.52886280891152282, 94.99999999999994316 ) ) ;
#6533 = ORIENTED_EDGE ( 'NONE', *, *, #14198, .F. ) ;
#6534 = CARTESIAN_POINT ( 'NONE',  ( -22.27502019258948707, 448.4948905683720568, 15.47720386886985189 ) ) ;
#6535 = CARTESIAN_POINT ( 'NONE',  ( -14.54375231895775222, 235.7448905765656093, 14.14213562373094568 ) ) ;
#6536 = EDGE_CURVE ( 'NONE', #18572, #16379, #13609, .T. ) ;
#6537 = ORIENTED_EDGE ( 'NONE', *, *, #6301, .T. ) ;
#6538 = CARTESIAN_POINT ( 'NONE',  ( -43.47609127650945737, 209.4774105891669933, 2.515022083182097745 ) ) ;
#6539 = CARTESIAN_POINT ( 'NONE',  ( -45.43829269268872650, 535.0573905683720568, -3.332260488124726194 ) ) ;
#6540 = ORIENTED_EDGE ( 'NONE', *, *, #17426, .T. ) ;
#6541 = CARTESIAN_POINT ( 'NONE',  ( -35.09675569278795848, 501.9948905683720000, -15.47720386886985544 ) ) ;
#6542 = DIRECTION ( 'NONE',  ( -1.000000000000000000, -0.000000000000000000, 0.000000000000000000 ) ) ;
#6543 = VECTOR ( 'NONE', #3761, 1000.000000000000000 ) ;
#6544 = CARTESIAN_POINT ( 'NONE',  ( -10.20829729246299422, 436.3698905765656377, 7.653668647301790529 ) ) ;
#6545 = CARTESIAN_POINT ( 'NONE',  ( -42.82802356641965957, 360.7448905765656377, -14.14213562373094746 ) ) ;
#6546 = CARTESIAN_POINT ( 'NONE',  ( -40.01497788969912506, 328.8073905601784759, 16.95518130045146776 ) ) ;
#6547 = CARTESIAN_POINT ( 'NONE',  ( -48.68588794268870146, 307.2448905601784759, 0.000000000000000000 ) ) ;
#6548 = CARTESIAN_POINT ( 'NONE',  ( 0.4033376246892518835, -4.059728990630810941, -5.968343123267134231 ) ) ;
#6549 = PLANE ( 'NONE',  #9111 ) ;
#6550 = CARTESIAN_POINT ( 'NONE',  ( 88.15330054274427596, 79.55187051032177692, -94.99999999999994316 ) ) ;
#6551 = LINE ( 'NONE', #3431, #17644 ) ;
#6552 = CARTESIAN_POINT ( 'NONE',  ( -45.43829269268869808, 315.0573905683720000, -3.332260488124726194 ) ) ;
#6553 = CARTESIAN_POINT ( 'NONE',  ( 2.416697501590669095, 217.7548513357008630, 45.00000000000000000 ) ) ;
#6554 = CARTESIAN_POINT ( 'NONE',  ( -8.685887942688712116, 272.2448905601784759, -2.449293598294705724E-15 ) ) ;
#6555 = LINE ( 'NONE', #13175, #21295 ) ;
#6556 = CARTESIAN_POINT ( 'NONE',  ( -32.01814843081344009, 287.5573905683719431, 16.75240474999999307 ) ) ;
#6557 = CARTESIAN_POINT ( 'NONE',  ( -42.88789093042845479, 506.3073905683720568, 9.489475012073734561 ) ) ;
#6558 = CARTESIAN_POINT ( 'NONE',  ( -14.54375231895776999, 363.4948905601784759, -14.14213562373094746 ) ) ;
#6559 = PLANE ( 'NONE',  #7354 ) ;
#6560 = ORIENTED_EDGE ( 'NONE', *, *, #18795, .T. ) ;
#6561 = CARTESIAN_POINT ( 'NONE',  ( -13.20868407381887444, 480.9948905683720000, -6.410867750099233042 ) ) ;
#6562 = CARTESIAN_POINT ( 'NONE',  ( 158.8141120573112630, 628.3356379279406383, -5.000000000000004441 ) ) ;
#6563 = CARTESIAN_POINT ( 'NONE',  ( -25.35362745456396993, 276.6823905683720000, 16.75240474999998952 ) ) ;
#6564 = EDGE_CURVE ( 'NONE', #12838, #21308, #3772, .T. ) ;
#6565 = ORIENTED_EDGE ( 'NONE', *, *, #1478, .F. ) ;
#6566 = CYLINDRICAL_SURFACE ( 'NONE', #6944, 21.20245194746113526 ) ;
#6567 = ADVANCED_FACE ( 'NONE', ( #17089 ), #13634, .T. ) ;
#6568 = CARTESIAN_POINT ( 'NONE',  ( -42.88789093042842637, 274.4323905683720568, -9.489475012073734561 ) ) ;
#6569 = CARTESIAN_POINT ( 'NONE',  ( -45.43829269268869808, 255.0573905683720000, -3.332260488124726638 ) ) ;
#6570 = CARTESIAN_POINT ( 'NONE',  ( -45.64106924314017277, 241.0573905765656093, -11.32908994701042715 ) ) ;
#6571 = VECTOR ( 'NONE', #18206, 1000.000000000000000 ) ;
#6572 = CARTESIAN_POINT ( 'NONE',  ( 60.03793209889851568, 10.52886280891152104, 136.1729372809869005 ) ) ;
#6573 = CARTESIAN_POINT ( 'NONE',  ( -14.48388495494898365, 229.8073905683720284, -9.489475012073734561 ) ) ;
#6574 = CARTESIAN_POINT ( 'NONE',  ( -44.16309181155855867, 274.4948905683720000, 6.410867750099241924 ) ) ;
#6575 = CARTESIAN_POINT ( 'NONE',  ( -11.93348319268872260, 380.3698905683720568, -2.051577885510841163E-15 ) ) ;
#6576 = CARTESIAN_POINT ( 'NONE',  ( -43.37414277151795261, 201.1719893629813498, 3.054701555947804792 ) ) ;
#6577 = AXIS2_PLACEMENT_3D ( 'NONE', #20707, #14231, #5880 ) ;
#6578 = VECTOR ( 'NONE', #19043, 1000.000000000000000 ) ;
#6579 = CARTESIAN_POINT ( 'NONE',  ( -24.70764059509556887, 459.1823905765656946, -19.99999999999999289 ) ) ;
#6580 = CARTESIAN_POINT ( 'NONE',  ( -28.68588794268875475, 600.7448905601785327, 0.000000000000000000 ) ) ;
#6581 = CARTESIAN_POINT ( 'NONE',  ( -11.93348319268872793, 418.8698905683720568, -2.051577885510841163E-15 ) ) ;
#6582 = CARTESIAN_POINT ( 'NONE',  ( -28.68588794268872633, 333.8848358243226357, 0.000000000000000000 ) ) ;
#6583 = EDGE_LOOP ( 'NONE', ( #10578, #13204 ) ) ;
#6584 = CARTESIAN_POINT ( 'NONE',  ( -10.20829729246299422, 432.8698905601784759, -7.653668647301794969 ) ) ;
#6585 = ORIENTED_EDGE ( 'NONE', *, *, #4721, .F. ) ;
#6586 = ORIENTED_EDGE ( 'NONE', *, *, #17304, .F. ) ;
#6587 = ORIENTED_EDGE ( 'NONE', *, *, #20816, .T. ) ;
#6588 = CARTESIAN_POINT ( 'NONE',  ( -42.83993802355417557, 205.8067832142903910, -4.966639429937480088 ) ) ;
#6589 = CARTESIAN_POINT ( 'NONE',  ( -28.68588794268870856, 314.7448905601785327, -19.99999999999999289 ) ) ;
#6590 = CARTESIAN_POINT ( 'NONE',  ( 0.000000000000000000, 0.000000000000000000, 0.000000000000000000 ) ) ;
#6591 = CARTESIAN_POINT ( 'NONE',  ( -38.17536295476244845, 346.9323905683720568, 14.20200298773971781 ) ) ;
#6592 = AXIS2_PLACEMENT_3D ( 'NONE', #622, #9028, #7082 ) ;
#6593 = MECHANICAL_DESIGN_GEOMETRIC_PRESENTATION_REPRESENTATION (  '', ( #15253 ), #15206 ) ;
#6594 = CARTESIAN_POINT ( 'NONE',  ( -47.16347859291445843, 491.3698905765655809, -7.653668647301793193 ) ) ;
#6595 = CARTESIAN_POINT ( 'NONE',  ( -45.43829269268871229, 363.8698905683720000, 0.000000000000000000 ) ) ;
#6596 = CARTESIAN_POINT ( 'NONE',  ( -45.43829269268869098, 225.6823905683720568, 3.332260488124734632 ) ) ;
#6597 = CARTESIAN_POINT ( 'NONE',  ( -14.48388495494900141, 387.9323905683720000, 9.489475012073731008 ) ) ;
#6598 = CARTESIAN_POINT ( 'NONE',  ( -28.68588794268870856, 299.4948905765656377, -19.99999999999999289 ) ) ;
#6599 = DIRECTION ( 'NONE',  ( -1.191790137725560488E-16, 1.000000000000000000, -0.000000000000000000 ) ) ;
#6600 = CARTESIAN_POINT ( 'NONE',  ( -22.27502019258947996, 290.7448905683720568, -15.47720386886985544 ) ) ;
#6601 = CARTESIAN_POINT ( 'NONE',  ( -28.68588794268874054, 573.2448905601785327, 0.000000000000000000 ) ) ;
#6602 = CARTESIAN_POINT ( 'NONE',  ( -13.20868407381886733, 429.7448905683720000, 6.410867750099229490 ) ) ;
#6603 = CARTESIAN_POINT ( 'NONE',  ( -42.82802356641965247, 285.9948905601784759, -14.14213562373094746 ) ) ;
#6604 = CARTESIAN_POINT ( 'NONE',  ( -42.82802356641968089, 515.9948905601785327, -14.14213562373094746 ) ) ;
#6605 = DIRECTION ( 'NONE',  ( -1.000000000000000000, 0.000000000000000000, 0.000000000000000000 ) ) ;
#6606 = CARTESIAN_POINT ( 'NONE',  ( -8.685887942688726326, 402.2448905601784759, -2.449293598294705724E-15 ) ) ;
#6607 = CARTESIAN_POINT ( 'NONE',  ( -44.16309181155857289, 354.7448905683720568, -6.410867750099231266 ) ) ;
#6608 = CARTESIAN_POINT ( 'NONE',  ( -11.93348319268873503, 478.8698905683720568, -2.051577885510841163E-15 ) ) ;
#6609 = CIRCLE ( 'NONE', #2833, 22.72497359561857877 ) ;
#6610 = ORIENTED_EDGE ( 'NONE', *, *, #11334, .T. ) ;
#6611 = CARTESIAN_POINT ( 'NONE',  ( -47.16347859291445843, 487.8698905601784759, 7.653668647301805628 ) ) ;
#6612 = CARTESIAN_POINT ( 'NONE',  ( -13.20868407381885135, 298.2448905683720000, 6.410867750099229490 ) ) ;
#6613 = ORIENTED_EDGE ( 'NONE', *, *, #1250, .T. ) ;
#6614 = LINE ( 'NONE', #156, #11507 ) ;
#6615 = ORIENTED_EDGE ( 'NONE', *, *, #10142, .T. ) ;
#6616 = CARTESIAN_POINT ( 'NONE',  ( -31.15442323855227968, 49.43082946763288277, 49.54048453831437371 ) ) ;
#6617 = ADVANCED_FACE ( 'NONE', ( #3880 ), #7437, .T. ) ;
#6618 = CARTESIAN_POINT ( 'NONE',  ( -42.88789093042844058, 396.3073905683720000, 9.489475012073734561 ) ) ;
#6619 = CARTESIAN_POINT ( 'NONE',  ( -47.16347859291445133, 442.6198905765656377, 7.653668647301805628 ) ) ;
#6620 = CYLINDRICAL_SURFACE ( 'NONE', #14218, 49.93977357075244328 ) ;
#6621 = CARTESIAN_POINT ( 'NONE',  ( -11.93348319268872793, 418.5573905683720568, 3.332260488124728415 ) ) ;
#6622 = CARTESIAN_POINT ( 'NONE',  ( -22.27502019258949773, 450.7448905683720000, -15.47720386886985544 ) ) ;
#6623 = APPLICATION_PROTOCOL_DEFINITION ( 'draft international standard', 'automotive_design', 1998, #9294 ) ;
#6624 = CARTESIAN_POINT ( 'NONE',  ( -8.685887942688859553, 401.9323905601783622, 3.978247347593479866 ) ) ;
#6625 = CARTESIAN_POINT ( 'NONE',  ( -24.70764059509556176, 369.1823905765655240, -19.99999999999999289 ) ) ;
#6626 = DIRECTION ( 'NONE',  ( -0.000000000000000000, -0.000000000000000000, -1.000000000000000000 ) ) ;
#6627 = CARTESIAN_POINT ( 'NONE',  ( -48.68588794268852382, 266.9323905601784190, -3.978247347593583783 ) ) ;
#6628 = CARTESIAN_POINT ( 'NONE',  ( 81.24038404635966515, 30.52886280891152282, -94.99999999999994316 ) ) ;
#6629 = CARTESIAN_POINT ( 'NONE',  ( -32.66413529028188378, 489.8073905765656377, -19.99999999999999289 ) ) ;
#6630 = CIRCLE ( 'NONE', #20459, 175.0000000000000284 ) ;
#6631 = CARTESIAN_POINT ( 'NONE',  ( -38.17536295476246266, 496.9323905683720568, 14.20200298773971781 ) ) ;
#6632 = FACE_OUTER_BOUND ( 'NONE', #5186, .T. ) ;
#6633 = DIRECTION ( 'NONE',  ( 1.000000000000000000, 0.000000000000000000, 0.000000000000000000 ) ) ;
#6634 = CARTESIAN_POINT ( 'NONE',  ( -42.88454851406326185, 206.4494888775581103, 4.837634058829628714 ) ) ;
#6635 = EDGE_CURVE ( 'NONE', #17719, #9040, #18287, .T. ) ;
#6636 = CARTESIAN_POINT ( 'NONE',  ( -28.68588794268872277, 412.8698905683720568, -16.75240474999999307 ) ) ;
#6637 = CARTESIAN_POINT ( 'NONE',  ( -48.68588794268872277, 461.9948905765656377, 0.000000000000000000 ) ) ;
#6638 = VECTOR ( 'NONE', #17466, 1000.000000000000000 ) ;
#6639 = CARTESIAN_POINT ( 'NONE',  ( -5.991983113971217634, 220.4588630705976584, -6.225382068641771127 ) ) ;
#6640 = CARTESIAN_POINT ( 'NONE',  ( -45.43829269268871229, 363.8698905683720000, 0.000000000000000000 ) ) ;
#6641 = ORIENTED_EDGE ( 'NONE', *, *, #4197, .F. ) ;
#6642 = CARTESIAN_POINT ( 'NONE',  ( -35.09675569278796559, 531.9948905683720568, -15.47720386886985544 ) ) ;
#6643 = ORIENTED_EDGE ( 'NONE', *, *, #12867, .T. ) ;
#6644 = CARTESIAN_POINT ( 'NONE',  ( -13.20868407381886911, 449.7448905683720000, 6.410867750099229490 ) ) ;
#6645 = CARTESIAN_POINT ( 'NONE',  ( -11.93348319268874036, 518.8698905683719431, -2.051577885510841163E-15 ) ) ;
#6646 = EDGE_LOOP ( 'NONE', ( #19343, #6992, #7626, #706, #10661, #15345 ) ) ;
#6647 = CARTESIAN_POINT ( 'NONE',  ( -14.54375231895777532, 430.9948905601784759, 14.14213562373094568 ) ) ;
#6648 = CARTESIAN_POINT ( 'NONE',  ( -14.48388495494901385, 479.8073905683720568, -9.489475012073736337 ) ) ;
#6649 = EDGE_LOOP ( 'NONE', ( #2705, #12545, #14143, #5633 ) ) ;
#6650 = CARTESIAN_POINT ( 'NONE',  ( -11.93348319268873858, 498.8698905683720000, -2.051577885510841163E-15 ) ) ;
#6651 = CARTESIAN_POINT ( 'NONE',  ( -11.50805310488956756, 52.75566815483727368, -46.53193503222628635 ) ) ;
#6652 = ADVANCED_FACE ( 'NONE', ( #872 ), #15686, .F. ) ;
#6653 = CARTESIAN_POINT ( 'NONE',  ( -45.64106924314020119, 452.9323905765656377, 11.32908994701042715 ) ) ;
#6654 = CARTESIAN_POINT ( 'NONE',  ( -47.16347859291444422, 361.3698905765655809, -7.653668647301793193 ) ) ;
#6655 = CYLINDRICAL_SURFACE ( 'NONE', #10262, 5.000000000000004441 ) ;
#6656 = PLANE ( 'NONE',  #19804 ) ;
#6657 = CARTESIAN_POINT ( 'NONE',  ( 20.42502041961814641, 163.4113008177049835, -60.00000000000000000 ) ) ;
#6658 = LINE ( 'NONE', #3002, #7037 ) ;
#6659 = CIRCLE ( 'NONE', #11856, 10.00000000000000178 ) ;
#6660 = SURFACE_SIDE_STYLE ('',( #19975 ) ) ;
#6661 = CARTESIAN_POINT ( 'NONE',  ( -28.68588794268873698, 10.52886280891152104, 0.000000000000000000 ) ) ;
#6662 =( BOUNDED_CURVE ( )  B_SPLINE_CURVE ( 2, ( #20752, #5306, #7430, #10893, #17292, #16896, #17500, #2476, #759, #7538, #15680, #2585, #20641, #11907, #7324, #13952, #20540 ),
 .UNSPECIFIED., .F., .T. ) 
 B_SPLINE_CURVE_WITH_KNOTS ( ( 3, 2, 2, 2, 2, 2, 2, 2, 3 ),
 ( 0.7031250000000002220, 0.7050781250000002220, 0.7070312500000002220, 0.7089843750000002220, 0.7109375000000002220, 0.7128906250000002220, 0.7148437500000002220, 0.7167968750000002220, 0.7187500000000002220 ),
 .UNSPECIFIED. ) 
 CURVE ( )  GEOMETRIC_REPRESENTATION_ITEM ( )  RATIONAL_B_SPLINE_CURVE ( ( 0.9999999999999977796, 0.9807852804032326510, 1.000000000000000000, 0.9807852804032304306, 1.000000000000000000, 0.9807852804032304306, 1.000000000000000000, 0.9807852804032304306, 1.000000000000000000, 0.9807852804032304306, 1.000000000000000000, 0.9807852804032304306, 1.000000000000000000, 0.9807852804032304306, 1.000000000000000000, 0.9807852804032282101, 1.000000000000002220 ) ) 
 REPRESENTATION_ITEM ( '' )  );
#6663 = CARTESIAN_POINT ( 'NONE',  ( -38.17536295476244845, 293.8073905683720568, -14.20200298773971426 ) ) ;
#6664 = ADVANCED_FACE ( 'NONE', ( #18692, #14063 ), #15470, .F. ) ;
#6665 = CARTESIAN_POINT ( 'NONE',  ( -11.73070664223723369, 233.1823905601784759, -11.32908994701042538 ) ) ;
#6666 = CARTESIAN_POINT ( 'NONE',  ( -32.66413529028186247, 275.0573905601784759, -19.99999999999999289 ) ) ;
#6667 = CARTESIAN_POINT ( 'NONE',  ( -11.73070664223725323, 416.0573905765656377, 11.32908994701042005 ) ) ;
#6668 = CARTESIAN_POINT ( 'NONE',  ( -25.35362745456397349, 298.1823905683720000, 16.75240474999998952 ) ) ;
#6669 = AXIS2_PLACEMENT_3D ( 'NONE', #1857, #1743, #18483 ) ;
#6670 = CARTESIAN_POINT ( 'NONE',  ( -42.88789093042844769, 504.4323905683720568, -9.489475012073734561 ) ) ;
#6671 = VECTOR ( 'NONE', #7077, 1000.000000000000000 ) ;
#6672 = DIRECTION ( 'NONE',  ( 1.000000000000000000, 0.000000000000000000, 0.000000000000000000 ) ) ;
#6673 = VERTEX_POINT ( 'NONE', #7220 ) ;
#6674 = CARTESIAN_POINT ( 'NONE',  ( -42.88789093042844769, 474.4323905683721136, -9.489475012073736337 ) ) ;
#6675 = SURFACE_STYLE_FILL_AREA ( #19767 ) ;
#6676 = CARTESIAN_POINT ( 'NONE',  ( -44.16309181155856578, 273.2448905683720568, -6.410867750099231266 ) ) ;
#6677 = VERTEX_POINT ( 'NONE', #18800 ) ;
#6678 = DIRECTION ( 'NONE',  ( -1.000000000000000000, 0.000000000000000000, 0.000000000000000000 ) ) ;
#6679 = CARTESIAN_POINT ( 'NONE',  ( -25.35362745456396638, 258.1823905683720000, 16.75240474999998952 ) ) ;
#6680 = AXIS2_PLACEMENT_3D ( 'NONE', #3938, #7282, #2753 ) ;
#6681 = CARTESIAN_POINT ( 'NONE',  ( -47.16347859291443001, 252.6198905765656377, 7.653668647301805628 ) ) ;
#6682 = LINE ( 'NONE', #2152, #5511 ) ;
#6683 = CARTESIAN_POINT ( 'NONE',  ( -47.16347859291443001, 237.8698905601784759, 7.653668647301805628 ) ) ;
#6684 = PLANE ( 'NONE',  #21300 ) ;
#6685 = CARTESIAN_POINT ( 'NONE',  ( -42.88789093042842637, 272.9323905683720568, -9.489475012073736337 ) ) ;
#6686 = VECTOR ( 'NONE', #4303, 1000.000000000000000 ) ;
#6687 = AXIS2_PLACEMENT_3D ( 'NONE', #10778, #5916, #12527 ) ;
#6688 = CARTESIAN_POINT ( 'NONE',  ( -35.09675569278794427, 363.4948905683720568, -15.47720386886985544 ) ) ;
#6689 = CARTESIAN_POINT ( 'NONE',  ( -42.82802356641967378, 505.9948905601785327, -14.14213562373094746 ) ) ;
#6690 = LINE ( 'NONE', #11673, #8647 ) ;
#6691 = EDGE_CURVE ( 'NONE', #19361, #18296, #16916, .T. ) ;
#6692 = CARTESIAN_POINT ( 'NONE',  ( -11.93348319268872970, 428.5573905683720568, 3.332260488124728415 ) ) ;
#6693 = CARTESIAN_POINT ( 'NONE',  ( -17.35679799567830628, 510.6823905601784759, 16.95518130045146421 ) ) ;
#6694 = VERTEX_POINT ( 'NONE', #4732 ) ;
#6695 = CARTESIAN_POINT ( 'NONE',  ( -17.35679799567829917, 420.6823905601784190, 16.95518130045146421 ) ) ;
#6696 = EDGE_LOOP ( 'NONE', ( #5586, #1291, #4710, #19263 ) ) ;
#6697 = CARTESIAN_POINT ( 'NONE',  ( 0.000000000000000000, 5.629165124598846326, -3.250000000000007550 ) ) ;
#6698 = ORIENTED_EDGE ( 'NONE', *, *, #18960, .F. ) ;
#6699 = ORIENTED_EDGE ( 'NONE', *, *, #9663, .T. ) ;
#6700 = CARTESIAN_POINT ( 'NONE',  ( -8.685887942688715668, 312.5573905601784190, -3.978247347593165895 ) ) ;
#6701 = DIRECTION ( 'NONE',  ( -0.000000000000000000, 0.000000000000000000, -1.000000000000000000 ) ) ;
#6702 = AXIS2_PLACEMENT_3D ( 'NONE', #18407, #5109, #7143 ) ;
#6703 = EDGE_CURVE ( 'NONE', #18883, #15214, #9281, .T. ) ;
#6704 = CARTESIAN_POINT ( 'NONE',  ( -28.68588794268871212, 342.8698905683720000, -16.75240474999999307 ) ) ;
#6705 = ORIENTED_EDGE ( 'NONE', *, *, #19806, .T. ) ;
#6706 = CARTESIAN_POINT ( 'NONE',  ( -42.82802356641967378, 480.7448905765655809, -14.14213562373094746 ) ) ;
#6707 = CARTESIAN_POINT ( 'NONE',  ( -35.09675569278794427, 361.9948905683720568, -15.47720386886985544 ) ) ;
#6708 = ADVANCED_FACE ( 'NONE', ( #7968 ), #20870, .T. ) ;
#6709 = CARTESIAN_POINT ( 'NONE',  ( -16.84014894278199037, 377.6198905683720568, 11.84573899990672530 ) ) ;
#6710 = ADVANCED_FACE ( 'NONE', ( #11005 ), #3015, .F. ) ;
#6711 = CARTESIAN_POINT ( 'NONE',  ( -42.82802356641965247, 310.7448905765656377, -14.14213562373094746 ) ) ;
#6712 = FACE_OUTER_BOUND ( 'NONE', #15476, .T. ) ;
#6713 = CARTESIAN_POINT ( 'NONE',  ( -35.09675569278793006, 261.9948905683720000, -15.47720386886985544 ) ) ;
#6714 = CARTESIAN_POINT ( 'NONE',  ( -8.685887942688712116, 272.2448905601784759, -2.449293598294705724E-15 ) ) ;
#6715 = CARTESIAN_POINT ( 'NONE',  ( -11.93348319268872970, 430.3698905683720568, -2.051577885510841163E-15 ) ) ;
#6716 = CARTESIAN_POINT ( 'NONE',  ( -21.03221929538691271, 284.1198905601784759, -18.47759065022572855 ) ) ;
#6717 = CARTESIAN_POINT ( 'NONE',  ( -48.68588794268872277, 497.2448905601785327, 0.000000000000000000 ) ) ;
#6718 = PLANE ( 'NONE',  #12658 ) ;
#6719 = DIRECTION ( 'NONE',  ( 1.000000000000000000, 0.000000000000000000, 0.000000000000000000 ) ) ;
#6720 = EDGE_CURVE ( 'NONE', #13843, #12838, #13253, .T. ) ;
#6721 = CARTESIAN_POINT ( 'NONE',  ( -11.93348319268871904, 340.3698905683720000, -2.051577885510841163E-15 ) ) ;
#6722 = CARTESIAN_POINT ( 'NONE',  ( -35.09675569278795848, 491.9948905683720568, -15.47720386886985544 ) ) ;
#6723 = ORIENTED_EDGE ( 'NONE', *, *, #17374, .T. ) ;
#6724 = CARTESIAN_POINT ( 'NONE',  ( -11.73070664223726212, 491.3073905601784190, 11.32908994701042005 ) ) ;
#6725 = CARTESIAN_POINT ( 'NONE',  ( -25.35362745456397349, 306.6823905683720000, 16.75240474999998952 ) ) ;
#6726 = ORIENTED_EDGE ( 'NONE', *, *, #17290, .T. ) ;
#6727 = FACE_OUTER_BOUND ( 'NONE', #6269, .T. ) ;
#6728 = VERTEX_POINT ( 'NONE', #4315 ) ;
#6729 = CARTESIAN_POINT ( 'NONE',  ( -32.69803402958404348, 51.81231153067828643, 49.43888967890881503 ) ) ;
#6730 = CARTESIAN_POINT ( 'NONE',  ( -40.53162694259544452, 394.1198905683720000, -11.84573899990672707 ) ) ;
#6731 = CARTESIAN_POINT ( 'NONE',  ( -10.20829729246299955, 481.6198905601785327, 7.653668647301790529 ) ) ;
#6732 = FILL_AREA_STYLE_COLOUR ( '', #7270 ) ;
#6733 = CARTESIAN_POINT ( 'NONE',  ( -22.27502019258948351, 426.9948905683720568, 15.47720386886985189 ) ) ;
#6734 = CARTESIAN_POINT ( 'NONE',  ( -22.27502019258947286, 252.2448905683720284, -15.47720386886985544 ) ) ;
#6735 = CARTESIAN_POINT ( 'NONE',  ( -14.48388495494900674, 437.9323905683720000, 9.489475012073731008 ) ) ;
#6736 = CARTESIAN_POINT ( 'NONE',  ( -6.276925316985672687, 600.7448905601785327, -44.69718552705352721 ) ) ;
#6737 = CARTESIAN_POINT ( 'NONE',  ( -42.82802356641965957, 360.7448905765656377, -14.14213562373094746 ) ) ;
#6738 = CARTESIAN_POINT ( 'NONE',  ( -15.09323033528205116, 47.79017490167774440, 47.70849690890445771 ) ) ;
#6739 = CARTESIAN_POINT ( 'NONE',  ( -10.20829729246298889, 387.6198905765655809, -7.653668647301794969 ) ) ;
#6740 = PLANE ( 'NONE',  #12906 ) ;
#6741 = CARTESIAN_POINT ( 'NONE',  ( -28.68588794268872633, 333.8848358243226357, 0.000000000000000000 ) ) ;
#6742 = CARTESIAN_POINT ( 'NONE',  ( -22.27502019258950128, 502.2448905683720568, -15.47720386886985544 ) ) ;
#6743 = CARTESIAN_POINT ( 'NONE',  ( 0.000000000000000000, 0.000000000000000000, 0.000000000000000000 ) ) ;
#6744 = CARTESIAN_POINT ( 'NONE',  ( -45.64106924314019409, 466.3073905601785327, -11.32908994701042538 ) ) ;
#6745 = CARTESIAN_POINT ( 'NONE',  ( -42.82802356641963826, 205.4725094246604442, 5.000000000000000888 ) ) ;
#6746 = CARTESIAN_POINT ( 'NONE',  ( -22.27502019258948351, 408.4948905683720000, 15.47720386886985189 ) ) ;
#6747 = CARTESIAN_POINT ( 'NONE',  ( -14.54375231895778420, 468.2448905765656377, -14.14213562373094746 ) ) ;
#6748 = CARTESIAN_POINT ( 'NONE',  ( -25.35362745456397349, 222.5573905683720568, -16.75240474999999307 ) ) ;
#6749 = CARTESIAN_POINT ( 'NONE',  ( -19.19641293061498644, 370.4323905683720000, -14.20200298773971603 ) ) ;
#6750 = ORIENTED_EDGE ( 'NONE', *, *, #10787, .T. ) ;
#6751 = CARTESIAN_POINT ( 'NONE',  ( -14.48388495494901740, 517.9323905683720568, 9.489475012073732785 ) ) ;
#6752 = VERTEX_POINT ( 'NONE', #2915 ) ;
#6753 = CARTESIAN_POINT ( 'NONE',  ( -40.53162694259544452, 446.6198905683720568, 11.84573899990672885 ) ) ;
#6754 = CARTESIAN_POINT ( 'NONE',  ( -16.84014894278200458, 517.6198905683719431, 11.84573899990672530 ) ) ;
#6755 = ORIENTED_EDGE ( 'NONE', *, *, #15009, .T. ) ;
#6756 = CARTESIAN_POINT ( 'NONE',  ( -24.70764059509557953, 529.1823905765656946, -19.99999999999999289 ) ) ;
#6757 = CARTESIAN_POINT ( 'NONE',  ( -45.43829269268871940, 494.1823905683720000, 3.332260488124734632 ) ) ;
#6758 = ORIENTED_EDGE ( 'NONE', *, *, #11205, .T. ) ;
#6759 = CARTESIAN_POINT ( 'NONE',  ( -25.35362745456399836, 496.6823905683721136, 16.75240474999998952 ) ) ;
#6760 = CARTESIAN_POINT ( 'NONE',  ( -10.20829729246300133, 491.6198905601784759, 7.653668647301790529 ) ) ;
#6761 = EDGE_CURVE ( 'NONE', #15845, #17381, #1862, .T. ) ;
#6762 = CARTESIAN_POINT ( 'NONE',  ( -32.66413529028188378, 414.1823905765656946, 19.99999999999999289 ) ) ;
#6763 = CARTESIAN_POINT ( 'NONE',  ( -45.64106924314017988, 361.0573905765656377, -11.32908994701042538 ) ) ;
#6764 = DIRECTION ( 'NONE',  ( -3.836511174089486173E-16, 0.000000000000000000, 1.000000000000000000 ) ) ;
#6765 = DIRECTION ( 'NONE',  ( 0.000000000000000000, 0.000000000000000000, -1.000000000000000000 ) ) ;
#6766 = DIRECTION ( 'NONE',  ( -1.000000000000000000, -0.000000000000000000, -0.000000000000000000 ) ) ;
#6767 = DIRECTION ( 'NONE',  ( -0.000000000000000000, -0.000000000000000000, 1.000000000000000000 ) ) ;
#6768 = CARTESIAN_POINT ( 'NONE',  ( -40.01497788969914637, 493.5573905765655809, 16.95518130045146776 ) ) ;
#6769 = CARTESIAN_POINT ( 'NONE',  ( -16.84014894278198327, 291.6198905683720000, -11.84573899990672707 ) ) ;
#6770 = CARTESIAN_POINT ( 'NONE',  ( 292.4526463419396691, 308.2087638784415162, 20.00000000000000355 ) ) ;
#6771 = CARTESIAN_POINT ( 'NONE',  ( -45.64106924314017277, 268.1823905601785327, 11.32908994701042715 ) ) ;
#6772 = CARTESIAN_POINT ( 'NONE',  ( -33.70050622342144209, 54.95587029918029742, -49.34681548815472496 ) ) ;
#6773 = CARTESIAN_POINT ( 'NONE',  ( -42.88789093042842637, 296.3073905683720000, 9.489475012073736337 ) ) ;
#6774 = EDGE_CURVE ( 'NONE', #11578, #9304, #18758, .T. ) ;
#6775 = CARTESIAN_POINT ( 'NONE',  ( -48.68588794268872988, 537.2448905601785327, 0.000000000000000000 ) ) ;
#6776 = CARTESIAN_POINT ( 'NONE',  ( -14.48388495494901385, 499.4323905683720000, 9.489475012073731008 ) ) ;
#6777 = AXIS2_PLACEMENT_3D ( 'NONE', #7800, #17658, #10840 ) ;
#6778 = CARTESIAN_POINT ( 'NONE',  ( -21.03221929538691626, 314.1198905601784759, -18.47759065022572855 ) ) ;
#6779 = ORIENTED_EDGE ( 'NONE', *, *, #17085, .T. ) ;
#6780 = CARTESIAN_POINT ( 'NONE',  ( -19.19641293061499354, 468.8073905683720000, 14.20200298773971426 ) ) ;
#6781 = CYLINDRICAL_SURFACE ( 'NONE', #14591, 38.00000000000000000 ) ;
#6782 = CARTESIAN_POINT ( 'NONE',  ( -11.93348319268870839, 258.8698905683720000, -2.051577885510841163E-15 ) ) ;
#6783 = ORIENTED_EDGE ( 'NONE', *, *, #12630, .F. ) ;
#6784 = FACE_OUTER_BOUND ( 'NONE', #7816, .T. ) ;
#6785 = EDGE_CURVE ( 'NONE', #17432, #14968, #21073, .T. ) ;
#6786 = AXIS2_PLACEMENT_3D ( 'NONE', #15464, #12207, #18794 ) ;
#6787 = CARTESIAN_POINT ( 'NONE',  ( -22.27502019258947286, 252.2448905683720284, -15.47720386886985544 ) ) ;
#6788 = CARTESIAN_POINT ( 'NONE',  ( -8.685887942688708563, 246.6823905765656377, 3.978247347593161010 ) ) ;
#6789 = DIRECTION ( 'NONE',  ( 0.000000000000000000, -1.000000000000000000, -1.155626614413199331E-16 ) ) ;
#6790 = CARTESIAN_POINT ( 'NONE',  ( -24.70764059509554755, 234.4323905601785043, -19.99999999999999289 ) ) ;
#6791 = CARTESIAN_POINT ( 'NONE',  ( -40.53162694259543031, 275.1198905683720568, 11.84573899990672885 ) ) ;
#6792 = CARTESIAN_POINT ( 'NONE',  ( -11.93348319268871904, 350.3698905683720568, -2.051577885510841163E-15 ) ) ;
#6793 = AXIS2_PLACEMENT_3D ( 'NONE', #16823, #11622, #9987 ) ;
#6794 = CARTESIAN_POINT ( 'NONE',  ( 81.24038404635966515, 30.52886280891152282, -94.99999999999994316 ) ) ;
#6795 = CARTESIAN_POINT ( 'NONE',  ( 115.7989814974898337, 152.5259582928263740, 20.00000000000000355 ) ) ;
#6796 = AXIS2_PLACEMENT_3D ( 'NONE', #10408, #18526, #13781 ) ;
#6797 = CARTESIAN_POINT ( 'NONE',  ( -16.84014894278199392, 417.6198905683720000, 11.84573899990672530 ) ) ;
#6798 = CARTESIAN_POINT ( 'NONE',  ( -45.64106924314017988, 341.0573905765656946, -11.32908994701042538 ) ) ;
#6799 = VERTEX_POINT ( 'NONE', #4528 ) ;
#6800 = CARTESIAN_POINT ( 'NONE',  ( -24.70764059509556532, 404.4323905601785327, -19.99999999999999289 ) ) ;
#6801 = ORIENTED_EDGE ( 'NONE', *, *, #11277, .F. ) ;
#6802 = CARTESIAN_POINT ( 'NONE',  ( 0.4053525175235877520, 3.145852061455921778, -6.500000000000000000 ) ) ;
#6803 = ORIENTED_EDGE ( 'NONE', *, *, #10400, .F. ) ;
#6804 = CARTESIAN_POINT ( 'NONE',  ( -28.68588794268873698, 532.8698905683719431, -16.75240474999999307 ) ) ;
#6805 = CARTESIAN_POINT ( 'NONE',  ( -11.73070664223723902, 301.3073905601784759, 11.32908994701042005 ) ) ;
#6806 = CARTESIAN_POINT ( 'NONE',  ( -43.63240380007614050, 209.9813597091836641, -1.306460585600322188 ) ) ;
#6807 = ORIENTED_EDGE ( 'NONE', *, *, #9452, .F. ) ;
#6808 = CARTESIAN_POINT ( 'NONE',  ( -28.68588794268871212, 322.8698905683720000, -16.75240474999999307 ) ) ;
#6809 = AXIS2_PLACEMENT_3D ( 'NONE', #2896, #19428, #12521 ) ;
#6810 = ORIENTED_EDGE ( 'NONE', *, *, #11651, .T. ) ;
#6811 = CARTESIAN_POINT ( 'NONE',  ( -16.84014894278198682, 357.6198905683720000, 11.84573899990672530 ) ) ;
#6812 = CARTESIAN_POINT ( 'NONE',  ( -32.01814843081344719, 376.0573905683720000, 16.75240474999999307 ) ) ;
#6813 = VECTOR ( 'NONE', #13112, 1000.000000000000000 ) ;
#6814 = CARTESIAN_POINT ( 'NONE',  ( -32.66413529028186957, 309.8073905765656377, -19.99999999999999289 ) ) ;
#6815 = CARTESIAN_POINT ( 'NONE',  ( 78.68120802659203150, 149.7457237375499517, -20.00000000000000355 ) ) ;
#6816 = CARTESIAN_POINT ( 'NONE',  ( -32.01814843081343298, 261.6823905683720568, -16.75240474999999307 ) ) ;
#6817 = CARTESIAN_POINT ( 'NONE',  ( 14.09825962131072785, 160.1716627696692683, 25.00000000000000000 ) ) ;
#6818 = CARTESIAN_POINT ( 'NONE',  ( -38.17536295476245556, 416.9323905683720568, 14.20200298773971781 ) ) ;
#6819 = CARTESIAN_POINT ( 'NONE',  ( 158.8141120573112630, 610.7448905601785327, 0.000000000000000000 ) ) ;
#6820 = CARTESIAN_POINT ( 'NONE',  ( -36.33955658999052929, 499.1198905601784759, 18.47759065022572500 ) ) ;
#6821 = DIRECTION ( 'NONE',  ( -1.191790137725560488E-16, 1.000000000000000000, -0.000000000000000000 ) ) ;
#6822 = CARTESIAN_POINT ( 'NONE',  ( -21.03221929538691626, 410.3698905601784759, 18.47759065022572500 ) ) ;
#6823 = CARTESIAN_POINT ( 'NONE',  ( -14.48388495494899253, 319.4323905683720568, 9.489475012073732785 ) ) ;
#6824 = CARTESIAN_POINT ( 'NONE',  ( -13.20868407381887621, 489.4948905683720568, -6.410867750099233042 ) ) ;
#6825 = EDGE_CURVE ( 'NONE', #445, #8097, #1393, .T. ) ;
#6826 = VERTEX_POINT ( 'NONE', #2700 ) ;
#6827 = CARTESIAN_POINT ( 'NONE',  ( -11.73070664223725856, 461.3073905601784759, 11.32908994701042005 ) ) ;
#6828 = CARTESIAN_POINT ( 'NONE',  ( -35.09675569278794427, 295.7448905683720568, 15.47720386886985366 ) ) ;
#6829 = EDGE_LOOP ( 'NONE', ( #5736, #954, #5902, #16079, #10977 ) ) ;
#6830 = CARTESIAN_POINT ( 'NONE',  ( 10.41669750159067220, 172.9933428177121471, 49.99999999999999289 ) ) ;
#6831 = ORIENTED_EDGE ( 'NONE', *, *, #14518, .T. ) ;
#6832 = DIRECTION ( 'NONE',  ( -0.000000000000000000, -1.000000000000000000, -0.000000000000000000 ) ) ;
#6833 = CARTESIAN_POINT ( 'NONE',  ( -13.20868407381886378, 390.9948905683720568, -6.410867750099233042 ) ) ;
#6834 = CARTESIAN_POINT ( 'NONE',  ( -11.73070664223726034, 481.3073905601785896, 11.32908994701042005 ) ) ;
#6835 = LINE ( 'NONE', #20042, #3152 ) ;
#6836 = CARTESIAN_POINT ( 'NONE',  ( -38.17536295476246266, 432.3073905683720000, -14.20200298773971426 ) ) ;
#6837 = CARTESIAN_POINT ( 'NONE',  ( -32.01814843081343298, 257.5573905683720568, 16.75240474999999307 ) ) ;
#6838 = CARTESIAN_POINT ( 'NONE',  ( -38.17536295476246266, 422.3073905683720000, -14.20200298773971426 ) ) ;
#6839 = APPLICATION_PROTOCOL_DEFINITION ( 'draft international standard', 'automotive_design', 1998, #11918 ) ;
#6840 = LINE ( 'NONE', #16237, #21035 ) ;
#6841 = EDGE_CURVE ( 'NONE', #10209, #5504, #4608, .T. ) ;
#6842 = CARTESIAN_POINT ( 'NONE',  ( -8.685887942688720997, 357.3073905765656377, -3.978247347593165895 ) ) ;
#6843 = CARTESIAN_POINT ( 'NONE',  ( -17.35679799567828496, 273.8073905601784759, -16.95518130045146421 ) ) ;
#6844 = PLANE ( 'NONE',  #15819 ) ;
#6845 = CARTESIAN_POINT ( 'NONE',  ( -19.19641293061497578, 327.3073905683721136, 14.20200298773971426 ) ) ;
#6846 = DIRECTION ( 'NONE',  ( 0.000000000000000000, 0.000000000000000000, -1.000000000000000000 ) ) ;
#6847 = CARTESIAN_POINT ( 'NONE',  ( -45.43829269268871940, 485.0573905683720568, -3.332260488124726194 ) ) ;
#6848 = CARTESIAN_POINT ( 'NONE',  ( -8.685887942688820473, 436.6823905765655809, 3.978247347593374172 ) ) ;
#6849 = CARTESIAN_POINT ( 'NONE',  ( -28.68588794268872988, 464.7448905601784759, -19.99999999999999289 ) ) ;
#6850 = CARTESIAN_POINT ( 'NONE',  ( -43.68588794268869435, 210.1437886375728965, -2.161864096862809871E-19 ) ) ;
#6851 = CARTESIAN_POINT ( 'NONE',  ( -11.93348319268872437, 390.0573905683720568, 3.332260488124728415 ) ) ;
#6852 = CARTESIAN_POINT ( 'NONE',  ( -36.33955658999050087, 263.8698905765656377, 18.47759065022572500 ) ) ;
#6853 = CARTESIAN_POINT ( 'NONE',  ( -40.53162694259542320, 224.1198905683720000, -11.84573899990672707 ) ) ;
#6854 = CARTESIAN_POINT ( 'NONE',  ( -38.17536295476245556, 362.3073905683719431, -14.20200298773971426 ) ) ;
#6855 = CIRCLE ( 'NONE', #18946, 5.000000000000004441 ) ;
#6856 = ORIENTED_EDGE ( 'NONE', *, *, #113, .T. ) ;
#6857 = CARTESIAN_POINT ( 'NONE',  ( -42.88789093042845479, 514.8073905683720568, 9.489475012073736337 ) ) ;
#6858 = ORIENTED_EDGE ( 'NONE', *, *, #12606, .T. ) ;
#6859 = CARTESIAN_POINT ( 'NONE',  ( -16.84014894278199748, 439.1198905683720568, 11.84573899990672530 ) ) ;
#6860 = CARTESIAN_POINT ( 'NONE',  ( -40.53162694259545873, 522.6198905683720568, -11.84573899990672707 ) ) ;
#6861 = ORIENTED_EDGE ( 'NONE', *, *, #6246, .F. ) ;
#6862 = CARTESIAN_POINT ( 'NONE',  ( -11.73070664223725501, 431.3073905601785327, 11.32908994701042005 ) ) ;
#6863 = CARTESIAN_POINT ( 'NONE',  ( -22.27502019258950128, 490.7448905683720000, -15.47720386886985544 ) ) ;
#6864 = EDGE_LOOP ( 'NONE', ( #18490, #12003, #12514, #20568, #123, #7663, #10814, #6252 ) ) ;
#6865 = CARTESIAN_POINT ( 'NONE',  ( -35.09675569278795848, 491.9948905683720568, -15.47720386886985544 ) ) ;
#6866 = CARTESIAN_POINT ( 'NONE',  ( -17.27797297620858430, 46.45732233689483337, -48.27343946592336010 ) ) ;
#6867 = CARTESIAN_POINT ( 'NONE',  ( -47.16347859291445133, 422.6198905765656377, 7.653668647301805628 ) ) ;
#6868 = CARTESIAN_POINT ( 'NONE',  ( 0.000000000000000000, 0.000000000000000000, 0.000000000000000000 ) ) ;
#6869 = CARTESIAN_POINT ( 'NONE',  ( -14.54375231895776288, 330.9948905601784190, 14.14213562373094568 ) ) ;
#6870 = CARTESIAN_POINT ( 'NONE',  ( -47.16347859291445133, 441.3698905765656377, -7.653668647301793193 ) ) ;
#6871 = LINE ( 'NONE', #15333, #2518 ) ;
#6872 = CARTESIAN_POINT ( 'NONE',  ( 0.4037800551813791605, -7.199367570657613236, -0.5303295852573151059 ) ) ;
#6873 = VECTOR ( 'NONE', #18625, 1000.000000000000000 ) ;
#6874 = CARTESIAN_POINT ( 'NONE',  ( 78.68120802659203150, 149.7457237375499517, 20.00000000000000355 ) ) ;
#6875 = CARTESIAN_POINT ( 'NONE',  ( -42.88695301665256920, 203.8419814082757568, -4.830353110044838694 ) ) ;
#6876 = CARTESIAN_POINT ( 'NONE',  ( -40.53162694259543031, 304.1198905683720000, -11.84573899990672707 ) ) ;
#6877 = CARTESIAN_POINT ( 'NONE',  ( -10.20829729246297113, 232.8698905601784759, -7.653668647301794969 ) ) ;
#6878 = CARTESIAN_POINT ( 'NONE',  ( -47.16347859291443712, 277.8698905601784759, 7.653668647301805628 ) ) ;
#6879 = CARTESIAN_POINT ( 'NONE',  ( -33.81853030400259996, 55.90295019273428068, -49.33467926027583417 ) ) ;
#6880 = CARTESIAN_POINT ( 'NONE',  ( -45.43829269268869808, 295.6823905683720000, 3.332260488124734632 ) ) ;
#6881 = EDGE_LOOP ( 'NONE', ( #10630, #2759, #6885, #17090 ) ) ;
#6882 = CARTESIAN_POINT ( 'NONE',  ( -8.685887942688712116, 272.2448905601784759, -2.449293598294705724E-15 ) ) ;
#6883 = CARTESIAN_POINT ( 'NONE',  ( -44.16309181155857999, 495.9948905683720568, 6.410867750099241924 ) ) ;
#6884 = CIRCLE ( 'NONE', #9646, 15.00000000000000355 ) ;
#6885 = ORIENTED_EDGE ( 'NONE', *, *, #15192, .F. ) ;
#6886 = CARTESIAN_POINT ( 'NONE',  ( -25.35362745456399480, 468.1823905683721136, 16.75240474999998952 ) ) ;
#6887 = EDGE_CURVE ( 'NONE', #11943, #8642, #19122, .T. ) ;
#6888 = DIRECTION ( 'NONE',  ( -0.000000000000000000, -1.000000000000000000, -0.000000000000000000 ) ) ;
#6889 = CARTESIAN_POINT ( 'NONE',  ( -32.01814843081343298, 256.0573905683720000, 16.75240474999999307 ) ) ;
#6890 = ORIENTED_EDGE ( 'NONE', *, *, #14397, .T. ) ;
#6891 = CARTESIAN_POINT ( 'NONE',  ( -17.35679799567828496, 335.4323905765656377, 16.95518130045146421 ) ) ;
#6892 = CARTESIAN_POINT ( 'NONE',  ( -45.43829269268869808, 245.6823905683720568, 3.332260488124734632 ) ) ;
#6893 = CARTESIAN_POINT ( 'NONE',  ( -36.33955658999050087, 243.8698905765656093, 18.47759065022572500 ) ) ;
#6894 = CARTESIAN_POINT ( 'NONE',  ( -47.16347859291445133, 421.3698905765656377, -7.653668647301793193 ) ) ;
#6895 = CARTESIAN_POINT ( 'NONE',  ( -24.70764059509554045, 224.4323905601784759, -19.99999999999999289 ) ) ;
#6896 = CARTESIAN_POINT ( 'NONE',  ( -16.84014894278197616, 257.6198905683720568, 11.84573899990672530 ) ) ;
#6897 = CARTESIAN_POINT ( 'NONE',  ( -32.01814843081344719, 363.1823905683720568, -16.75240474999999307 ) ) ;
#6898 = CARTESIAN_POINT ( 'NONE',  ( -11.73070664223726745, 503.1823905601785327, -11.32908994701042538 ) ) ;
#6899 = ADVANCED_FACE ( 'NONE', ( #16428 ), #6559, .F. ) ;
#6900 = CARTESIAN_POINT ( 'NONE',  ( -11.93348319268872615, 408.8698905683720568, -2.051577885510841163E-15 ) ) ;
#6901 = DIRECTION ( 'NONE',  ( 0.000000000000000000, 0.000000000000000000, 1.000000000000000000 ) ) ;
#6902 = CIRCLE ( 'NONE', #19005, 40.00000000000000000 ) ;
#6903 = EDGE_LOOP ( 'NONE', ( #8636, #14114, #13505, #19365, #10872, #20519, #6907 ) ) ;
#6904 = CARTESIAN_POINT ( 'NONE',  ( -10.20829729246299067, 412.8698905601784759, -7.653668647301794969 ) ) ;
#6905 = ORIENTED_EDGE ( 'NONE', *, *, #15663, .T. ) ;
#6906 = CYLINDRICAL_SURFACE ( 'NONE', #9433, 20.00000000000000000 ) ;
#6907 = ORIENTED_EDGE ( 'NONE', *, *, #15009, .F. ) ;
#6908 = EDGE_LOOP ( 'NONE', ( #15554, #20119, #13420, #15263 ) ) ;
#6909 = CARTESIAN_POINT ( 'NONE',  ( -45.43829269268872650, 535.0573905683720568, -3.332260488124726194 ) ) ;
#6910 = CARTESIAN_POINT ( 'NONE',  ( -11.73070664223724080, 283.1823905601784759, -11.32908994701042715 ) ) ;
#6911 = CARTESIAN_POINT ( 'NONE',  ( 51.50493485826542184, 141.8799693780962912, 20.00000000000000355 ) ) ;
#6912 = CARTESIAN_POINT ( 'NONE',  ( -40.53162694259543031, 326.6198905683720568, 11.84573899990672885 ) ) ;
#6913 = CARTESIAN_POINT ( 'NONE',  ( -22.27502019258947641, 356.9948905683720000, 15.47720386886985189 ) ) ;
#6914 = CARTESIAN_POINT ( 'NONE',  ( -11.93348319268872260, 359.1823905683720568, -3.332260488124732856 ) ) ;
#6915 = EDGE_CURVE ( 'NONE', #18327, #16131, #19939, .T. ) ;
#6916 = CARTESIAN_POINT ( 'NONE',  ( -32.66413529028186957, 294.1823905765655809, 19.99999999999999289 ) ) ;
#6917 = CIRCLE ( 'NONE', #16961, 5.000000000000004441 ) ;
#6918 = LINE ( 'NONE', #559, #15542 ) ;
#6919 = CARTESIAN_POINT ( 'NONE',  ( -22.27502019258946220, 256.9948905683720568, 15.47720386886985189 ) ) ;
#6920 = AXIS2_PLACEMENT_3D ( 'NONE', #13297, #7788, #4956 ) ;
#6921 = CARTESIAN_POINT ( 'NONE',  ( -44.16309181155857289, 415.9948905683720000, 6.410867750099241924 ) ) ;
#6922 = CARTESIAN_POINT ( 'NONE',  ( -30.69714544437698933, 48.92315038370448121, 121.1724415244209894 ) ) ;
#6923 = DIRECTION ( 'NONE',  ( 1.000000000000000000, 0.000000000000000000, 0.000000000000000000 ) ) ;
#6924 = CARTESIAN_POINT ( 'NONE',  ( -14.54375231895775578, 275.7448905765656377, 14.14213562373094568 ) ) ;
#6925 = VECTOR ( 'NONE', #3316, 1000.000000000000000 ) ;
#6926 = DIRECTION ( 'NONE',  ( -0.3090169943749472292, 0.000000000000000000, 0.9510565162951536422 ) ) ;
#6927 = EDGE_CURVE ( 'NONE', #3730, #19453, #606, .T. ) ;
#6928 = CARTESIAN_POINT ( 'NONE',  ( -35.09675569278795138, 337.2448905683720568, 15.47720386886985366 ) ) ;
#6929 = CARTESIAN_POINT ( 'NONE',  ( -13.20868407381887089, 458.2448905683720568, 6.410867750099229490 ) ) ;
#6930 = ORIENTED_EDGE ( 'NONE', *, *, #16959, .F. ) ;
#6931 = CARTESIAN_POINT ( 'NONE',  ( -47.16347859291445843, 466.6198905601784759, -7.653668647301793193 ) ) ;
#6932 = CARTESIAN_POINT ( 'NONE',  ( -38.17536295476244135, 295.4323905683720000, 14.20200298773971781 ) ) ;
#6933 = VERTEX_POINT ( 'NONE', #21281 ) ;
#6934 = VECTOR ( 'NONE', #14245, 1000.000000000000000 ) ;
#6935 = VECTOR ( 'NONE', #1905, 1000.000000000000000 ) ;
#6936 = CARTESIAN_POINT ( 'NONE',  ( -40.01497788969913216, 343.5573905765655240, 16.95518130045146776 ) ) ;
#6937 = ORIENTED_EDGE ( 'NONE', *, *, #6825, .T. ) ;
#6938 = DIRECTION ( 'NONE',  ( -0.000000000000000000, 0.000000000000000000, -1.000000000000000000 ) ) ;
#6939 = CARTESIAN_POINT ( 'NONE',  ( -16.84014894278199392, 381.6198905683720568, -11.84573899990672707 ) ) ;
#6940 = DIRECTION ( 'NONE',  ( -1.000000000000000000, -0.000000000000000000, -0.000000000000000000 ) ) ;
#6941 = PLANE ( 'NONE',  #10389 ) ;
#6942 = CARTESIAN_POINT ( 'NONE',  ( -19.19641293061498999, 427.3073905683720568, 14.20200298773971426 ) ) ;
#6943 = CARTESIAN_POINT ( 'NONE',  ( -13.20868407381884779, 250.9948905683720284, -6.410867750099233042 ) ) ;
#6944 = AXIS2_PLACEMENT_3D ( 'NONE', #13187, #18144, #14203 ) ;
#6945 = CARTESIAN_POINT ( 'NONE',  ( -40.53162694259544452, 425.1198905683720000, 11.84573899990672885 ) ) ;
#6946 = APPLICATION_PROTOCOL_DEFINITION ( 'draft international standard', 'automotive_design', 1998, #14970 ) ;
#6947 = CARTESIAN_POINT ( 'NONE',  ( -48.68588794268887909, 397.5573905601784190, 3.978247347592742678 ) ) ;
#6948 = CARTESIAN_POINT ( 'NONE',  ( -36.33955658999051508, 353.8698905765656377, 18.47759065022572500 ) ) ;
#6949 = CARTESIAN_POINT ( 'NONE',  ( -123.2946569474810161, 10.52886280891152104, 20.57735571454641388 ) ) ;
#6950 = DIRECTION ( 'NONE',  ( -1.191790137725560488E-16, 1.000000000000000000, -0.000000000000000000 ) ) ;
#6951 = CARTESIAN_POINT ( 'NONE',  ( -45.43829269268870519, 324.1823905683720000, 3.332260488124734632 ) ) ;
#6952 = CARTESIAN_POINT ( 'NONE',  ( -48.68588794268870856, 371.9948905765655809, 0.000000000000000000 ) ) ;
#6953 = CARTESIAN_POINT ( 'NONE',  ( -22.27502019258949773, 472.2448905683720568, -15.47720386886985544 ) ) ;
#6954 = DIRECTION ( 'NONE',  ( -1.000000000000000000, -0.000000000000000000, -0.000000000000000000 ) ) ;
#6955 = AXIS2_PLACEMENT_3D ( 'NONE', #2594, #9173, #11118 ) ;
#6956 = CARTESIAN_POINT ( 'NONE',  ( -48.68588794268870146, 307.2448905601784759, 0.000000000000000000 ) ) ;
#6957 = CARTESIAN_POINT ( 'NONE',  ( -13.20868407381886200, 389.7448905683720000, 6.410867750099229490 ) ) ;
#6958 = CARTESIAN_POINT ( 'NONE',  ( -24.70764059509553690, 264.8073905765656377, 19.99999999999998934 ) ) ;
#6959 = EDGE_CURVE ( 'NONE', #15181, #573, #8180, .T. ) ;
#6960 = CARTESIAN_POINT ( 'NONE',  ( -24.70764059509557242, 530.0573905601785327, 19.99999999999998934 ) ) ;
#6961 = CARTESIAN_POINT ( 'NONE',  ( -13.20868407381885845, 358.2448905683720000, 6.410867750099229490 ) ) ;
#6962 = EDGE_CURVE ( 'NONE', #9177, #20205, #9705, .T. ) ;
#6963 = ORIENTED_EDGE ( 'NONE', *, *, #15543, .F. ) ;
#6964 = CARTESIAN_POINT ( 'NONE',  ( -45.43829269268873361, 523.8698905683720568, 0.000000000000000000 ) ) ;
#6965 = ORIENTED_EDGE ( 'NONE', *, *, #10809, .T. ) ;
#6966 = CARTESIAN_POINT ( 'NONE',  ( -28.68588794268873698, 531.3698905683720568, -16.75240474999999307 ) ) ;
#6967 = ORIENTED_EDGE ( 'NONE', *, *, #15708, .T. ) ;
#6968 = DIRECTION ( 'NONE',  ( -1.000000000000000000, 0.000000000000000000, 0.000000000000000000 ) ) ;
#6969 = CARTESIAN_POINT ( 'NONE',  ( -11.93348319268873681, 488.8698905683720568, -2.051577885510841163E-15 ) ) ;
#6970 = ORIENTED_EDGE ( 'NONE', *, *, #15650, .F. ) ;
#6971 = CARTESIAN_POINT ( 'NONE',  ( -22.27502019258950128, 490.7448905683720000, -15.47720386886985544 ) ) ;
#6972 = CARTESIAN_POINT ( 'NONE',  ( 88.28695088269886071, 142.5259582928263455, 40.00000000000000000 ) ) ;
#6973 = EDGE_CURVE ( 'NONE', #19853, #18701, #3831, .T. ) ;
#6974 = CARTESIAN_POINT ( 'NONE',  ( -28.68588794268871922, 424.4948905765656377, 19.99999999999999289 ) ) ;
#6975 = CARTESIAN_POINT ( 'NONE',  ( -8.685887942688449215, 297.3073905765655809, -3.978247347592526850 ) ) ;
#6976 = CARTESIAN_POINT ( 'NONE',  ( -36.33955658999050797, 299.1198905601785327, 18.47759065022572500 ) ) ;
#6977 = CARTESIAN_POINT ( 'NONE',  ( -48.68588794268865882, 441.6823905765655809, -3.978247347593264927 ) ) ;
#6978 = PLANE ( 'NONE',  #9757 ) ;
#6979 =( BOUNDED_CURVE ( )  B_SPLINE_CURVE ( 2, ( #8546, #356, #10376, #12010, #10588, #10693, #16889, #2388, #460, #3685, #781, #5832, #12333, #18496, #2497, #17209, #16999 ),
 .UNSPECIFIED., .F., .T. ) 
 B_SPLINE_CURVE_WITH_KNOTS ( ( 3, 2, 2, 2, 2, 2, 2, 2, 3 ),
 ( 0.2031250000000001665, 0.2050781250000001665, 0.2070312500000001665, 0.2089843750000001665, 0.2109375000000001665, 0.2128906250000001943, 0.2148437500000001943, 0.2167968750000001943, 0.2187500000000001943 ),
 .UNSPECIFIED. ) 
 CURVE ( )  GEOMETRIC_REPRESENTATION_ITEM ( )  RATIONAL_B_SPLINE_CURVE ( ( 0.9999999999999983347, 0.9807852804032320959, 1.000000000000000000, 0.9807852804032304306, 1.000000000000000000, 0.9807852804032304306, 1.000000000000000000, 0.9807852804032304306, 1.000000000000000000, 0.9807852804032304306, 1.000000000000000000, 0.9807852804032304306, 1.000000000000000000, 0.9807852804032304306, 1.000000000000000000, 0.9807852804032285432, 1.000000000000001998 ) ) 
 REPRESENTATION_ITEM ( '' )  );
#6980 = EDGE_CURVE ( 'NONE', #4584, #8426, #19721, .T. ) ;
#6981 = PRESENTATION_STYLE_ASSIGNMENT (( #1930 ) ) ;
#6982 = LINE ( 'NONE', #17160, #19035 ) ;
#6983 = CARTESIAN_POINT ( 'NONE',  ( -11.93348319268871549, 300.6823905683720568, -3.332260488124732856 ) ) ;
#6984 = DIRECTION ( 'NONE',  ( 0.000000000000000000, 1.000000000000000000, 0.000000000000000000 ) ) ;
#6985 = CARTESIAN_POINT ( 'NONE',  ( -42.88789093042844058, 444.4323905683720568, -9.489475012073736337 ) ) ;
#6986 = CARTESIAN_POINT ( 'NONE',  ( -48.68588794268871567, 411.9948905765656377, 0.000000000000000000 ) ) ;
#6987 = CARTESIAN_POINT ( 'NONE',  ( -42.88789093042841927, 266.3073905683720000, 9.489475012073736337 ) ) ;
#6988 = EDGE_CURVE ( 'NONE', #604, #7438, #7017, .T. ) ;
#6989 = ORIENTED_EDGE ( 'NONE', *, *, #7093, .T. ) ;
#6990 = DIRECTION ( 'NONE',  ( 0.000000000000000000, -0.000000000000000000, 1.000000000000000000 ) ) ;
#6991 = CARTESIAN_POINT ( 'NONE',  ( -40.53162694259545162, 494.1198905683720000, -11.84573899990672707 ) ) ;
#6992 = ORIENTED_EDGE ( 'NONE', *, *, #440, .T. ) ;
#6993 = CARTESIAN_POINT ( 'NONE',  ( -40.53162694259545162, 474.1198905683720568, -11.84573899990672707 ) ) ;
#6994 = DIRECTION ( 'NONE',  ( 0.000000000000000000, 0.000000000000000000, -1.000000000000000000 ) ) ;
#6995 = CARTESIAN_POINT ( 'NONE',  ( -16.84014894278197971, 270.1198905683720568, -11.84573899990672707 ) ) ;
#6996 = ORIENTED_EDGE ( 'NONE', *, *, #17769, .F. ) ;
#6997 = DIRECTION ( 'NONE',  ( 0.4627175328665442677, 0.000000000000000000, -0.8865057725575724579 ) ) ;
#6998 = CARTESIAN_POINT ( 'NONE',  ( 105.7989814974898479, 152.5259582928263740, -20.00000000000000355 ) ) ;
#6999 = CARTESIAN_POINT ( 'NONE',  ( -11.93348319268870661, 250.3698905683720000, -2.051577885510841163E-15 ) ) ;
#7000 = CARTESIAN_POINT ( 'NONE',  ( -48.68588794268887199, 307.5573905601784759, 3.978247347592742678 ) ) ;
#7001 = DIRECTION ( 'NONE',  ( -1.000000000000000000, 0.000000000000000000, 0.000000000000000000 ) ) ;
#7002 = CARTESIAN_POINT ( 'NONE',  ( -11.93348319268871016, 258.5573905683720568, 3.332260488124728415 ) ) ;
#7003 = CARTESIAN_POINT ( 'NONE',  ( -19.19641293061498288, 358.8073905683720000, 14.20200298773971426 ) ) ;
#7004 = CARTESIAN_POINT ( 'NONE',  ( 20.42502041961813930, 230.5765313837437418, 60.00000000000000000 ) ) ;
#7005 = EDGE_CURVE ( 'NONE', #13483, #11839, #21325, .T. ) ;
#7006 = VECTOR ( 'NONE', #19540, 1000.000000000000000 ) ;
#7007 = CARTESIAN_POINT ( 'NONE',  ( -45.43829269268871940, 403.8698905683720000, 0.000000000000000000 ) ) ;
#7008 = CARTESIAN_POINT ( 'NONE',  ( -28.68588794268872633, 333.8848358243226357, 0.000000000000000000 ) ) ;
#7009 = CARTESIAN_POINT ( 'NONE',  ( -48.68588794268871567, 407.2448905601784759, 0.000000000000000000 ) ) ;
#7010 = ORIENTED_EDGE ( 'NONE', *, *, #9347, .T. ) ;
#7011 = FACE_OUTER_BOUND ( 'NONE', #2271, .T. ) ;
#7012 = EDGE_LOOP ( 'NONE', ( #17895, #9415, #8615, #20147 ) ) ;
#7013 = ORIENTED_EDGE ( 'NONE', *, *, #12867, .F. ) ;
#7014 = CARTESIAN_POINT ( 'NONE',  ( -38.17536295476247687, 533.8073905683720568, -14.20200298773971426 ) ) ;
#7015 = CARTESIAN_POINT ( 'NONE',  ( -17.35679799567829207, 293.8073905601784759, -16.95518130045146421 ) ) ;
#7016 = CARTESIAN_POINT ( 'NONE',  ( -45.64106924314017277, 321.0573905765656377, -11.32908994701042538 ) ) ;
#7017 = CIRCLE ( 'NONE', #19127, 49.93977357075243617 ) ;
#7018 = CARTESIAN_POINT ( 'NONE',  ( -45.43829269268870519, 315.6823905683720000, 3.332260488124734632 ) ) ;
#7019 = ORIENTED_EDGE ( 'NONE', *, *, #8089, .T. ) ;
#7020 = CARTESIAN_POINT ( 'NONE',  ( -14.48388495494899786, 349.8073905683720000, -9.489475012073736337 ) ) ;
#7021 = CIRCLE ( 'NONE', #9096, 4.000000000000001776 ) ;
#7022 = CARTESIAN_POINT ( 'NONE',  ( -38.17536295476245556, 362.3073905683719431, -14.20200298773971426 ) ) ;
#7023 = EDGE_CURVE ( 'NONE', #2702, #8292, #9781, .T. ) ;
#7024 = CARTESIAN_POINT ( 'NONE',  ( -24.70764059509554045, 304.8073905765656377, 19.99999999999998934 ) ) ;
#7025 = CARTESIAN_POINT ( 'NONE',  ( 30.42502041961814996, 170.1716627696692683, -20.00000000000000355 ) ) ;
#7026 = CARTESIAN_POINT ( 'NONE',  ( -19.19641293061497223, 260.4323905683720568, -14.20200298773971603 ) ) ;
#7027 = CARTESIAN_POINT ( 'NONE',  ( -43.15185836128295449, 202.0883771310974169, 3.971358459629988236 ) ) ;
#7028 = CARTESIAN_POINT ( 'NONE',  ( -45.43829269268871940, 415.3698905683720568, 0.000000000000000000 ) ) ;
#7029 = CARTESIAN_POINT ( 'NONE',  ( -26.36214243864212037, 46.04536198394939106, 122.1890418585359015 ) ) ;
#7030 = CARTESIAN_POINT ( 'NONE',  ( -40.01497788969915348, 503.5573905765656946, 16.95518130045146776 ) ) ;
#7031 = FACE_OUTER_BOUND ( 'NONE', #2777, .T. ) ;
#7032 = CARTESIAN_POINT ( 'NONE',  ( -14.48388495494899608, 331.3073905683720000, -9.489475012073736337 ) ) ;
#7033 = CARTESIAN_POINT ( 'NONE',  ( -11.93348319268873503, 469.1823905683719431, -3.332260488124732856 ) ) ;
#7034 = ORIENTED_EDGE ( 'NONE', *, *, #8610, .F. ) ;
#7035 = CARTESIAN_POINT ( 'NONE',  ( -14.54375231895777887, 460.9948905601785327, 14.14213562373094568 ) ) ;
#7036 = CARTESIAN_POINT ( 'NONE',  ( -38.17536295476244845, 292.3073905683720000, -14.20200298773971426 ) ) ;
#7037 = VECTOR ( 'NONE', #21061, 1000.000000000000114 ) ;
#7038 = ADVANCED_FACE ( 'NONE', ( #211 ), #8805, .T. ) ;
#7039 = EDGE_LOOP ( 'NONE', ( #11206, #3750 ) ) ;
#7040 = CARTESIAN_POINT ( 'NONE',  ( -45.64106924314017988, 342.9323905765655240, 11.32908994701042538 ) ) ;
#7041 = VERTEX_POINT ( 'NONE', #14117 ) ;
#7042 = DIRECTION ( 'NONE',  ( 0.3090169943749472847, -0.000000000000000000, -0.9510565162951536422 ) ) ;
#7043 = CARTESIAN_POINT ( 'NONE',  ( -21.03221929538690560, 340.3698905601784759, 18.47759065022572500 ) ) ;
#7044 = CARTESIAN_POINT ( 'NONE',  ( -40.53162694259543031, 305.1198905683720000, 11.84573899990672885 ) ) ;
#7045 = CARTESIAN_POINT ( 'NONE',  ( -38.17536295476245556, 383.8073905683720568, -14.20200298773971426 ) ) ;
#7046 = CARTESIAN_POINT ( 'NONE',  ( -14.54375231895775045, 230.9948905601784759, 14.14213562373094568 ) ) ;
#7047 = CARTESIAN_POINT ( 'NONE',  ( -8.685887942688905738, 386.6823905765655240, 3.978247347593586447 ) ) ;
#7048 = CARTESIAN_POINT ( 'NONE',  ( -45.43829269268871940, 423.8698905683720568, 0.000000000000000000 ) ) ;
#7049 = CARTESIAN_POINT ( 'NONE',  ( -45.43829269268869098, 255.0573905683720000, -3.332260488124726194 ) ) ;
#7050 = CARTESIAN_POINT ( 'NONE',  ( -19.19641293061498644, 417.3073905683720568, 14.20200298773971426 ) ) ;
#7051 = PRODUCT_CONTEXT ( 'NONE', #3894, 'mechanical' ) ;
#7052 = EDGE_CURVE ( 'NONE', #4231, #4363, #7377, .T. ) ;
#7053 = CARTESIAN_POINT ( 'NONE',  ( -32.66413529028187668, 369.8073905765655240, -19.99999999999999289 ) ) ;
#7054 = CARTESIAN_POINT ( 'NONE',  ( -28.68588794268870501, 274.7448905601784759, -19.99999999999999289 ) ) ;
#7055 = CARTESIAN_POINT ( 'NONE',  ( -11.93348319268871727, 329.1823905683720568, -3.332260488124732856 ) ) ;
#7056 = CARTESIAN_POINT ( 'NONE',  ( -22.27502019258949062, 468.4948905683720000, 15.47720386886985189 ) ) ;
#7057 = CARTESIAN_POINT ( 'NONE',  ( 5.074999999999999289, 7.505553499465139389, 0.000000000000000000 ) ) ;
#7058 = CARTESIAN_POINT ( 'NONE',  ( -42.83955070047272073, 204.4880047785818533, -4.967744786903342202 ) ) ;
#7059 = CARTESIAN_POINT ( 'NONE',  ( -47.16347859291443712, 306.6198905601784759, -7.653668647301793193 ) ) ;
#7060 = CARTESIAN_POINT ( 'NONE',  ( -35.09675569278794427, 383.4948905683720000, -15.47720386886985544 ) ) ;
#7061 = DIRECTION ( 'NONE',  ( 1.000000000000000000, 0.000000000000000000, -0.000000000000000000 ) ) ;
#7062 = CARTESIAN_POINT ( 'NONE',  ( -45.64106924314020119, 536.3073905601785327, -11.32908994701042715 ) ) ;
#7063 = CARTESIAN_POINT ( 'NONE',  ( -40.53162694259543741, 345.1198905683720568, 11.84573899990672885 ) ) ;
#7064 = EDGE_LOOP ( 'NONE', ( #8965, #19966 ) ) ;
#7065 = CARTESIAN_POINT ( 'NONE',  ( -16.84014894278201169, 530.1198905683720568, -11.84573899990672707 ) ) ;
#7066 = ORIENTED_EDGE ( 'NONE', *, *, #11701, .F. ) ;
#7067 = CARTESIAN_POINT ( 'NONE',  ( -14.54375231895776466, 350.9948905601784759, 14.14213562373094568 ) ) ;
#7068 = CARTESIAN_POINT ( 'NONE',  ( -22.27502019258949773, 526.9948905683720568, 15.47720386886985189 ) ) ;
#7069 = CARTESIAN_POINT ( 'NONE',  ( -11.06088464903279878, 213.9102039777116602, -5.773301668816275267 ) ) ;
#7070 = CARTESIAN_POINT ( 'NONE',  ( -47.16347859291446554, 531.3698905765655809, -7.653668647301793193 ) ) ;
#7071 = CARTESIAN_POINT ( 'NONE',  ( -13.20868407381887444, 488.2448905683720000, 6.410867750099229490 ) ) ;
#7072 = ORIENTED_EDGE ( 'NONE', *, *, #2140, .T. ) ;
#7073 = CARTESIAN_POINT ( 'NONE',  ( -35.09675569278796559, 485.7448905683720568, 15.47720386886985366 ) ) ;
#7074 = CARTESIAN_POINT ( 'NONE',  ( -21.03221929538693047, 428.8698905765655809, -18.47759065022572855 ) ) ;
#7075 = DIRECTION ( 'NONE',  ( -1.000000000000000000, 0.000000000000000000, 0.000000000000000000 ) ) ;
#7076 = CARTESIAN_POINT ( 'NONE',  ( -42.82802356641965247, 298.4948905601784759, 14.14213562373094923 ) ) ;
#7077 = DIRECTION ( 'NONE',  ( 0.000000000000000000, -1.000000000000000000, 0.000000000000000000 ) ) ;
#7078 =( REPRESENTATION_RELATIONSHIP ('NONE','NONE', #1888, #8616 ) REPRESENTATION_RELATIONSHIP_WITH_TRANSFORMATION ( #8891 )SHAPE_REPRESENTATION_RELATIONSHIP( ) );
#7079 = CARTESIAN_POINT ( 'NONE',  ( 45.67500000000000426, 0.000000000000000000, 0.000000000000000000 ) ) ;
#7080 = LINE ( 'NONE', #7184, #9238 ) ;
#7081 = CARTESIAN_POINT ( 'NONE',  ( -40.01497788969914637, 435.6823905601784759, -16.95518130045146421 ) ) ;
#7082 = DIRECTION ( 'NONE',  ( 0.000000000000000000, 0.000000000000000000, 1.000000000000000000 ) ) ;
#7083 = CARTESIAN_POINT ( 'NONE',  ( -38.17536295476244135, 306.9323905683719431, 14.20200298773971781 ) ) ;
#7084 = CARTESIAN_POINT ( 'NONE',  ( 105.7989814974898479, 152.5259582928263740, -20.00000000000000355 ) ) ;
#7085 = CARTESIAN_POINT ( 'NONE',  ( -13.20868407381887089, 450.9948905683720000, -6.410867750099233042 ) ) ;
#7086 = CARTESIAN_POINT ( 'NONE',  ( -11.73070664223725501, 397.9323905765656377, -11.32908994701042538 ) ) ;
#7087 = CARTESIAN_POINT ( 'NONE',  ( -16.84014894278197616, 279.1198905683720568, 11.84573899990672530 ) ) ;
#7088 = EDGE_CURVE ( 'NONE', #15582, #445, #20595, .T. ) ;
#7089 = EDGE_LOOP ( 'NONE', ( #3966, #18540, #895, #14020, #4094, #7886 ) ) ;
#7090 = FACE_OUTER_BOUND ( 'NONE', #708, .T. ) ;
#7091 = CARTESIAN_POINT ( 'NONE',  ( -14.48388495494901385, 491.3073905683720000, -9.489475012073734561 ) ) ;
#7092 = EDGE_CURVE ( 'NONE', #2403, #12984, #7389, .T. ) ;
#7093 = EDGE_CURVE ( 'NONE', #5985, #2702, #4044, .T. ) ;
#7094 = EDGE_CURVE ( 'NONE', #13710, #1213, #20703, .T. ) ;
#7095 = ORIENTED_EDGE ( 'NONE', *, *, #6825, .F. ) ;
#7096 = CARTESIAN_POINT ( 'NONE',  ( -28.68588794268872633, 467.8698905683720000, 16.75240474999999307 ) ) ;
#7097 = DIRECTION ( 'NONE',  ( -0.1337298367054296222, 0.9910178256594273094, -0.000000000000000000 ) ) ;
#7098 = CARTESIAN_POINT ( 'NONE',  ( -38.17536295476244135, 252.3073905683720284, -14.20200298773971426 ) ) ;
#7099 = ORIENTED_EDGE ( 'NONE', *, *, #11004, .F. ) ;
#7100 =( BOUNDED_CURVE ( )  B_SPLINE_CURVE ( 2, ( #16445, #4856, #4968, #3033, #11451, #11239, #9616, #6471, #18155, #14720, #21200, #16552, #13086, #12977, #6, #19674, #1626 ),
 .UNSPECIFIED., .F., .T. ) 
 B_SPLINE_CURVE_WITH_KNOTS ( ( 3, 2, 2, 2, 2, 2, 2, 2, 3 ),
 ( 0.8125000000000002220, 0.8144531250000002220, 0.8164062500000002220, 0.8183593750000002220, 0.8203125000000002220, 0.8222656250000002220, 0.8242187500000002220, 0.8261718750000002220, 0.8281250000000002220 ),
 .UNSPECIFIED. ) 
 CURVE ( )  GEOMETRIC_REPRESENTATION_ITEM ( )  RATIONAL_B_SPLINE_CURVE ( ( 0.9999999999999977796, 0.9807852804032326510, 1.000000000000000000, 0.9807852804032304306, 1.000000000000000000, 0.9807852804032304306, 1.000000000000000000, 0.9807852804032304306, 1.000000000000000000, 0.9807852804032304306, 1.000000000000000000, 0.9807852804032304306, 1.000000000000000000, 0.9807852804032304306, 1.000000000000000000, 0.9807852804032282101, 1.000000000000002220 ) ) 
 REPRESENTATION_ITEM ( '' )  );
#7101 = CARTESIAN_POINT ( 'NONE',  ( 2.234578793975251082E-15, -5.788408252967910173, -2.974182810908600594 ) ) ;
#7102 = CARTESIAN_POINT ( 'NONE',  ( -8.685887942688735208, 476.9948905765656377, -2.449293598294705724E-15 ) ) ;
#7103 = DIRECTION ( 'NONE',  ( 1.000000000000000000, 0.000000000000000000, 0.000000000000000000 ) ) ;
#7104 = CARTESIAN_POINT ( 'NONE',  ( -13.20868407381884779, 240.9948905683720284, -6.410867750099233042 ) ) ;
#7105 = EDGE_CURVE ( 'NONE', #12056, #17482, #17146, .T. ) ;
#7106 = CARTESIAN_POINT ( 'NONE',  ( -32.66413529028187668, 419.8073905765655809, -19.99999999999999289 ) ) ;
#7107 = CARTESIAN_POINT ( 'NONE',  ( -47.16347859291443001, 236.6198905601784475, -7.653668647301793193 ) ) ;
#7108 = CARTESIAN_POINT ( 'NONE',  ( -16.84014894278197261, 237.6198905683720284, 11.84573899990672530 ) ) ;
#7109 = CARTESIAN_POINT ( 'NONE',  ( -35.09675569278795138, 367.2448905683720000, 15.47720386886985366 ) ) ;
#7110 = DIRECTION ( 'NONE',  ( 0.000000000000000000, 0.000000000000000000, -1.000000000000000000 ) ) ;
#7111 = CIRCLE ( 'NONE', #19221, 6.500000000000000888 ) ;
#7112 = CARTESIAN_POINT ( 'NONE',  ( -19.19641293061498644, 397.3073905683720000, 14.20200298773971426 ) ) ;
#7113 = CARTESIAN_POINT ( 'NONE',  ( -28.68588794268872988, 509.7448905601784759, 19.99999999999999289 ) ) ;
#7114 = CARTESIAN_POINT ( 'NONE',  ( -8.685887942688726326, 411.9323905601785896, 3.978247347593161010 ) ) ;
#7115 = CIRCLE ( 'NONE', #3341, 200.0000000000000000 ) ;
#7116 = ORIENTED_EDGE ( 'NONE', *, *, #13467, .T. ) ;
#7117 = CYLINDRICAL_SURFACE ( 'NONE', #16017, 19.99999999999999645 ) ;
#7118 = ORIENTED_EDGE ( 'NONE', *, *, #8627, .T. ) ;
#7119 = CARTESIAN_POINT ( 'NONE',  ( -22.27502019258949773, 528.4948905683719431, 15.47720386886985189 ) ) ;
#7120 = CARTESIAN_POINT ( 'NONE',  ( -47.16347859291443712, 287.8698905601784759, 7.653668647301805628 ) ) ;
#7121 = CARTESIAN_POINT ( 'NONE',  ( -43.47642916300955562, 209.4785612017895176, -2.513052019990858366 ) ) ;
#7122 = CARTESIAN_POINT ( 'NONE',  ( -16.84014894278198327, 319.1198905683720568, 11.84573899990672530 ) ) ;
#7123 = ORIENTED_EDGE ( 'NONE', *, *, #5957, .T. ) ;
#7124 = CARTESIAN_POINT ( 'NONE',  ( -14.48388495494899608, 347.9323905683720000, 9.489475012073732785 ) ) ;
#7125 = CARTESIAN_POINT ( 'NONE',  ( -11.93348319268872260, 368.8698905683720000, -2.051577885510841163E-15 ) ) ;
#7126 = CARTESIAN_POINT ( 'NONE',  ( -14.54375231895776110, 278.2448905765655809, -14.14213562373094746 ) ) ;
#7127 = CYLINDRICAL_SURFACE ( 'NONE', #10675, 5.000000000000001776 ) ;
#7128 = CARTESIAN_POINT ( 'NONE',  ( -16.84014894278197971, 260.1198905683720568, -11.84573899990672707 ) ) ;
#7129 = CARTESIAN_POINT ( 'NONE',  ( 60.03793209889851568, 30.52886280891152282, 126.1729372809868863 ) ) ;
#7130 = CARTESIAN_POINT ( 'NONE',  ( -16.84014894278199392, 409.1198905683720000, 11.84573899990672530 ) ) ;
#7131 = CIRCLE ( 'NONE', #19237, 4.000000000000000000 ) ;
#7132 = CARTESIAN_POINT ( 'NONE',  ( -47.16347859291444422, 336.6198905601784759, -7.653668647301793193 ) ) ;
#7133 = CARTESIAN_POINT ( 'NONE',  ( -32.66413529028186957, 355.0573905601785327, -19.99999999999999289 ) ) ;
#7134 = DIRECTION ( 'NONE',  ( 1.191790137725560488E-16, -1.000000000000000000, -0.000000000000000000 ) ) ;
#7135 = CARTESIAN_POINT ( 'NONE',  ( -42.88789093042842637, 324.4323905683719431, -9.489475012073736337 ) ) ;
#7136 = CARTESIAN_POINT ( 'NONE',  ( -11.93348319268873325, 458.5573905683720568, 3.332260488124728415 ) ) ;
#7137 = VERTEX_POINT ( 'NONE', #7597 ) ;
#7138 = CARTESIAN_POINT ( 'NONE',  ( -47.16347859291445843, 467.8698905601784759, 7.653668647301805628 ) ) ;
#7139 = CARTESIAN_POINT ( 'NONE',  ( -14.48388495494899075, 289.8073905683720000, -9.489475012073736337 ) ) ;
#7140 = EDGE_CURVE ( 'NONE', #11348, #10847, #2823, .T. ) ;
#7141 = EDGE_LOOP ( 'NONE', ( #13419, #5842, #14415 ) ) ;
#7142 = ORIENTED_EDGE ( 'NONE', *, *, #13867, .T. ) ;
#7143 = DIRECTION ( 'NONE',  ( 0.000000000000000000, -0.000000000000000000, 1.000000000000000000 ) ) ;
#7144 = CARTESIAN_POINT ( 'NONE',  ( -45.64106924314018698, 338.1823905601784759, 11.32908994701042715 ) ) ;
#7145 = CARTESIAN_POINT ( 'NONE',  ( -45.43829269268870519, 293.8698905683720568, 0.000000000000000000 ) ) ;
#7146 = VECTOR ( 'NONE', #15813, 1000.000000000000000 ) ;
#7147 = CARTESIAN_POINT ( 'NONE',  ( -45.43829269268871229, 375.3698905683720568, 0.000000000000000000 ) ) ;
#7148 = CARTESIAN_POINT ( 'NONE',  ( 52.60622592008805043, 10.52886280891152104, 151.0302712373927250 ) ) ;
#7149 = ADVANCED_FACE ( 'NONE', ( #10850, #15637, #17454, #12271, #2642 ), #20495, .F. ) ;
#7150 = CARTESIAN_POINT ( 'NONE',  ( -24.70764059509558308, 529.1823905765656946, -19.99999999999999289 ) ) ;
#7151 = CARTESIAN_POINT ( 'NONE',  ( -45.43829269268871229, 414.1823905683720000, 3.332260488124734632 ) ) ;
#7152 = CARTESIAN_POINT ( 'NONE',  ( -13.20868407381884779, 260.9948905683720568, -6.410867750099233042 ) ) ;
#7153 = CARTESIAN_POINT ( 'NONE',  ( -14.48388495494900674, 427.9323905683720568, 9.489475012073731008 ) ) ;
#7154 = ITEM_DEFINED_TRANSFORMATION ( 'NONE', 'NONE', #10019,  #12794 ) ;
#7155 = CARTESIAN_POINT ( 'NONE',  ( -28.68588794268870856, 334.4948905765656377, 19.99999999999999289 ) ) ;
#7156 = CARTESIAN_POINT ( 'NONE',  ( -48.68588794268873698, 573.2448905601785327, 0.000000000000000000 ) ) ;
#7157 = CARTESIAN_POINT ( 'NONE',  ( -44.16309181155857289, 333.2448905683720568, -6.410867750099231266 ) ) ;
#7158 = CARTESIAN_POINT ( 'NONE',  ( -11.93348319268873503, 480.3698905683720568, -2.051577885510841163E-15 ) ) ;
#7159 = DIRECTION ( 'NONE',  ( 0.000000000000000000, 0.000000000000000000, 1.000000000000000000 ) ) ;
#7160 = CARTESIAN_POINT ( 'NONE',  ( -43.52298375438361688, 200.6544955639567434, -2.225641045960684128 ) ) ;
#7161 = DIRECTION ( 'NONE',  ( -0.000000000000000000, -1.000000000000000000, -0.000000000000000000 ) ) ;
#7162 = CARTESIAN_POINT ( 'NONE',  ( -42.88789093042843348, 386.3073905683720000, 9.489475012073736337 ) ) ;
#7163 = CARTESIAN_POINT ( 'NONE',  ( -25.99280818006741356, 45.91387061696119076, -122.2681842339391523 ) ) ;
#7164 = CARTESIAN_POINT ( 'NONE',  ( -21.03221929538692692, 520.3698905601785327, 18.47759065022572500 ) ) ;
#7165 = CARTESIAN_POINT ( 'NONE',  ( -44.16309181155856578, 334.4948905683720568, 6.410867750099241924 ) ) ;
#7166 = EDGE_CURVE ( 'NONE', #6213, #8588, #14306, .T. ) ;
#7167 = VERTEX_POINT ( 'NONE', #5986 ) ;
#7168 = CARTESIAN_POINT ( 'NONE',  ( -11.93348319268873858, 498.8698905683720000, -2.051577885510841163E-15 ) ) ;
#7169 = ORIENTED_EDGE ( 'NONE', *, *, #17728, .T. ) ;
#7170 = CARTESIAN_POINT ( 'NONE',  ( -24.70764059509555111, 350.0573905601785327, 19.99999999999998934 ) ) ;
#7171 = CARTESIAN_POINT ( 'NONE',  ( -48.68588794268871567, 427.2448905601784759, 0.000000000000000000 ) ) ;
#7172 = CARTESIAN_POINT ( 'NONE',  ( -174.5421710038924061, 600.7448905601785327, 96.70028278950401557 ) ) ;
#7173 = CARTESIAN_POINT ( 'NONE',  ( -8.685887942688740537, 516.9948905765655809, -2.449293598294705724E-15 ) ) ;
#7174 = CARTESIAN_POINT ( 'NONE',  ( -42.88789093042844769, 464.8073905683720568, 9.489475012073736337 ) ) ;
#7175 = VERTEX_POINT ( 'NONE', #9119 ) ;
#7176 = CARTESIAN_POINT ( 'NONE',  ( -32.01814843081345430, 491.6823905683720568, -16.75240474999999307 ) ) ;
#7177 = CARTESIAN_POINT ( 'NONE',  ( -42.82802356641964536, 243.2448905765656093, 14.14213562373094923 ) ) ;
#7178 = CARTESIAN_POINT ( 'NONE',  ( -48.68588794268871567, 431.6823905765655809, -3.978247347593158345 ) ) ;
#7179 = DIRECTION ( 'NONE',  ( 0.000000000000000000, 0.9253149302858357794, 0.3791995250394160633 ) ) ;
#7180 = CARTESIAN_POINT ( 'NONE',  ( -43.68588794268869435, 188.9102039777116602, 0.000000000000000000 ) ) ;
#7181 = DIRECTION ( 'NONE',  ( 0.000000000000000000, 0.000000000000000000, 1.000000000000000000 ) ) ;
#7182 = DIRECTION ( 'NONE',  ( 0.000000000000000000, 0.000000000000000000, 1.000000000000000000 ) ) ;
#7183 = ADVANCED_FACE ( 'NONE', ( #19188 ), #17562, .F. ) ;
#7184 = CARTESIAN_POINT ( 'NONE',  ( -46.31968306282883674, 326.0737056351150613, 33.59072564020503648 ) ) ;
#7185 = CARTESIAN_POINT ( 'NONE',  ( -11.73070664223723192, 241.3073905601784759, 11.32908994701042005 ) ) ;
#7186 = DIRECTION ( 'NONE',  ( -0.6352526299242177155, 0.000000000000000000, -0.7723044064191041391 ) ) ;
#7187 = CARTESIAN_POINT ( 'NONE',  ( -22.27502019258947641, 272.2448905683720568, -15.47720386886985544 ) ) ;
#7188 = AXIS2_PLACEMENT_3D ( 'NONE', #5914, #9154, #2900 ) ;
#7189 = CARTESIAN_POINT ( 'NONE',  ( -42.82802356641964536, 258.4948905601784759, 14.14213562373094923 ) ) ;
#7190 = CARTESIAN_POINT ( 'NONE',  ( 60.03793209889851568, 30.52886280891152282, 136.1729372809869005 ) ) ;
#7191 = CARTESIAN_POINT ( 'NONE',  ( -11.93348319268873148, 450.6823905683721136, -3.332260488124732856 ) ) ;
#7192 = CARTESIAN_POINT ( 'NONE',  ( -14.54375231895777532, 398.2448905765655809, -14.14213562373094746 ) ) ;
#7193 = CARTESIAN_POINT ( 'NONE',  ( -44.16309181155856578, 274.7448905683720568, -6.410867750099231266 ) ) ;
#7194 = EDGE_CURVE ( 'NONE', #5288, #12191, #6084, .T. ) ;
#7195 = ORIENTED_EDGE ( 'NONE', *, *, #3786, .T. ) ;
#7196 = CARTESIAN_POINT ( 'NONE',  ( -45.64106924314016567, 268.1823905601785327, 11.32908994701042538 ) ) ;
#7197 = CARTESIAN_POINT ( 'NONE',  ( -16.84014894278200103, 479.1198905683720000, 11.84573899990672530 ) ) ;
#7198 = ORIENTED_EDGE ( 'NONE', *, *, #3976, .F. ) ;
#7199 = CARTESIAN_POINT ( 'NONE',  ( -42.82802356641966668, 410.7448905765656377, -14.14213562373094746 ) ) ;
#7200 = CARTESIAN_POINT ( 'NONE',  ( -22.27502019258946220, 256.9948905683720568, 15.47720386886985189 ) ) ;
#7201 = ORIENTED_EDGE ( 'NONE', *, *, #1104, .T. ) ;
#7202 = CARTESIAN_POINT ( 'NONE',  ( -8.685887942688720997, 336.9948905765656377, -2.449293598294705724E-15 ) ) ;
#7203 = VECTOR ( 'NONE', #12360, 1000.000000000000000 ) ;
#7204 = CARTESIAN_POINT ( 'NONE',  ( -47.16347859291445843, 482.6198905765656377, 7.653668647301805628 ) ) ;
#7205 = CARTESIAN_POINT ( 'NONE',  ( -10.20829729246298889, 391.6198905601784759, 7.653668647301790529 ) ) ;
#7206 = CARTESIAN_POINT ( 'NONE',  ( -38.55245932946841947, 223.9102039777118023, -13.63907185705690495 ) ) ;
#7207 = CARTESIAN_POINT ( 'NONE',  ( -28.68588794268870146, 252.8698905683720000, -16.75240474999999307 ) ) ;
#7208 = CARTESIAN_POINT ( 'NONE',  ( -44.16309181155858710, 525.9948905683720568, 6.410867750099241924 ) ) ;
#7209 = CARTESIAN_POINT ( 'NONE',  ( -45.64106924314017988, 372.9323905765656377, 11.32908994701042538 ) ) ;
#7210 = CARTESIAN_POINT ( 'NONE',  ( -25.35362745456397704, 251.0573905683720000, -16.75240474999999307 ) ) ;
#7211 = CARTESIAN_POINT ( 'NONE',  ( -45.43829269268870519, 345.6823905683720568, 3.332260488124734632 ) ) ;
#7212 = CARTESIAN_POINT ( 'NONE',  ( -47.16347859291443712, 317.8698905601784190, 7.653668647301805628 ) ) ;
#7213 = AXIS2_PLACEMENT_3D ( 'NONE', #10374, #5299, #15063 ) ;
#7214 = CARTESIAN_POINT ( 'NONE',  ( -42.88789093042844058, 394.8073905683720000, 9.489475012073736337 ) ) ;
#7215 = EDGE_CURVE ( 'NONE', #18669, #15822, #10475, .T. ) ;
#7216 =( BOUNDED_CURVE ( )  B_SPLINE_CURVE ( 2, ( #7849, #15776, #14476, #12524, #7529, #21059, #6228, #1377, #12842, #4301, #17491, #15994, #4408, #10988, #19432, #2680, #2999 ),
 .UNSPECIFIED., .F., .T. ) 
 B_SPLINE_CURVE_WITH_KNOTS ( ( 3, 2, 2, 2, 2, 2, 2, 2, 3 ),
 ( 0.5781250000000001110, 0.5800781250000001110, 0.5820312500000001110, 0.5839843750000001110, 0.5859375000000002220, 0.5878906250000002220, 0.5898437500000002220, 0.5917968750000002220, 0.5937500000000002220 ),
 .UNSPECIFIED. ) 
 CURVE ( )  GEOMETRIC_REPRESENTATION_ITEM ( )  RATIONAL_B_SPLINE_CURVE ( ( 0.9999999999999988898, 0.9807852804032315408, 1.000000000000000000, 0.9807852804032304306, 1.000000000000000000, 0.9807852804032304306, 1.000000000000000000, 0.9807852804032304306, 1.000000000000000000, 0.9807852804032304306, 1.000000000000000000, 0.9807852804032304306, 1.000000000000000000, 0.9807852804032304306, 1.000000000000000000, 0.9807852804032282101, 1.000000000000002220 ) ) 
 REPRESENTATION_ITEM ( '' )  );
#7217 = CARTESIAN_POINT ( 'NONE',  ( -28.68588794268871922, 409.7448905601784759, 19.99999999999999289 ) ) ;
#7218 = ADVANCED_FACE ( 'NONE', ( #2860 ), #17667, .T. ) ;
#7219 = ORIENTED_EDGE ( 'NONE', *, *, #1048, .F. ) ;
#7220 = CARTESIAN_POINT ( 'NONE',  ( -22.30770786884144741, 45.31613216062291372, -122.9933582338429687 ) ) ;
#7221 = ORIENTED_EDGE ( 'NONE', *, *, #13941, .F. ) ;
#7222 = EDGE_LOOP ( 'NONE', ( #2358, #15533, #17072, #317 ) ) ;
#7223 = CARTESIAN_POINT ( 'NONE',  ( -25.35362745456400901, 502.5573905683719431, -16.75240474999999307 ) ) ;
#7224 = CARTESIAN_POINT ( 'NONE',  ( -24.70764059509555466, 294.4323905601784759, -19.99999999999999289 ) ) ;
#7225 = DIRECTION ( 'NONE',  ( 0.000000000000000000, 0.000000000000000000, 1.000000000000000000 ) ) ;
#7226 = EDGE_LOOP ( 'NONE', ( #714, #5366, #6807, #2509 ) ) ;
#7227 = CARTESIAN_POINT ( 'NONE',  ( -35.09675569278794427, 327.2448905683720000, 15.47720386886985366 ) ) ;
#7228 = PRODUCT_DEFINITION ( 'UNKNOWN', '', #10726, #17212 ) ;
#7229 = ORIENTED_EDGE ( 'NONE', *, *, #4299, .F. ) ;
#7230 = CARTESIAN_POINT ( 'NONE',  ( -42.88789093042843348, 342.9323905683721136, -9.489475012073736337 ) ) ;
#7231 = CARTESIAN_POINT ( 'NONE',  ( -11.93348319268872260, 348.5573905683720568, 3.332260488124728859 ) ) ;
#7232 = CARTESIAN_POINT ( 'NONE',  ( -14.54375231895776110, 288.2448905765656377, -14.14213562373094746 ) ) ;
#7233 = DIRECTION ( 'NONE',  ( -1.191790137725560488E-16, 1.000000000000000000, -0.000000000000000000 ) ) ;
#7234 = CARTESIAN_POINT ( 'NONE',  ( -45.43829269268869808, 254.1823905683720000, 3.332260488124734632 ) ) ;
#7235 = DIRECTION ( 'NONE',  ( 0.000000000000000000, 0.000000000000000000, 1.000000000000000000 ) ) ;
#7236 = CARTESIAN_POINT ( 'NONE',  ( -40.53162694259544452, 414.1198905683720000, -11.84573899990672707 ) ) ;
#7237 = CARTESIAN_POINT ( 'NONE',  ( -27.39625443478472278, 46.47175521496745176, 121.9628765649355415 ) ) ;
#7238 = CARTESIAN_POINT ( 'NONE',  ( -40.01497788969915348, 450.4323905765656377, -16.95518130045146421 ) ) ;
#7239 = PLANE ( 'NONE',  #2179 ) ;
#7240 = CARTESIAN_POINT ( 'NONE',  ( -40.53162694259543741, 334.1198905683720568, -11.84573899990672707 ) ) ;
#7241 = CARTESIAN_POINT ( 'NONE',  ( -22.27502019258949773, 470.7448905683720568, -15.47720386886985544 ) ) ;
#7242 = EDGE_LOOP ( 'NONE', ( #17088, #4041, #18357, #13154 ) ) ;
#7243 = CARTESIAN_POINT ( 'NONE',  ( -32.66413529028189089, 465.0573905601784759, -19.99999999999999289 ) ) ;
#7244 = CARTESIAN_POINT ( 'NONE',  ( -32.01814843081344009, 286.0573905683720568, 16.75240474999999307 ) ) ;
#7245 = ORIENTED_EDGE ( 'NONE', *, *, #12879, .F. ) ;
#7246 = AXIS2_PLACEMENT_3D ( 'NONE', #13624, #3763, #862 ) ;
#7247 = LINE ( 'NONE', #18826, #12567 ) ;
#7248 = CARTESIAN_POINT ( 'NONE',  ( -13.20868407381886733, 439.7448905683720000, 6.410867750099229490 ) ) ;
#7249 = ORIENTED_EDGE ( 'NONE', *, *, #20021, .F. ) ;
#7250 = LINE ( 'NONE', #476, #9472 ) ;
#7251 = CARTESIAN_POINT ( 'NONE',  ( -42.82802356641965957, 345.9948905601784759, -14.14213562373094746 ) ) ;
#7252 = CARTESIAN_POINT ( 'NONE',  ( -42.88789093042842637, 302.9323905683720568, -9.489475012073736337 ) ) ;
#7253 = CARTESIAN_POINT ( 'NONE',  ( -40.53162694259543741, 384.1198905683720568, -11.84573899990672707 ) ) ;
#7254 = VECTOR ( 'NONE', #4504, 1000.000000000000000 ) ;
#7255 = CARTESIAN_POINT ( 'NONE',  ( -11.73070664223724968, 373.1823905601784759, -11.32908994701042538 ) ) ;
#7256 = B_SPLINE_CURVE_WITH_KNOTS ( 'NONE', 3,
 ( #9788, #19747, #4817, #14372, #2996, #18121 ),
 .UNSPECIFIED., .F., .F.,
 ( 4, 2, 4 ),
 ( 2.380733003136581732E-07, 0.001898835937927382872, 0.003797433802554452380 ),
 .UNSPECIFIED. ) ;
#7257 = CARTESIAN_POINT ( 'NONE',  ( -32.66413529028189799, 519.8073905765655809, -19.99999999999999289 ) ) ;
#7258 = CARTESIAN_POINT ( 'NONE',  ( -25.35362745456398414, 396.6823905683720000, 16.75240474999998952 ) ) ;
#7259 = CARTESIAN_POINT ( 'NONE',  ( -32.01814843081343298, 237.5573905683720568, 16.75240474999999307 ) ) ;
#7260 = CLOSED_SHELL ( 'NONE', ( #18867, #17030, #4911, #3382, #5068, #9607, #16001, #19201, #9611, #12315, #6708, #9995, #7668, #11293, #6168, #18655, #10599, #18430, #10265, #18334, #20210, #10260, #1554, #122, #17813, #1050, #2428 ) ) ;
#7261 = CARTESIAN_POINT ( 'NONE',  ( -11.93348319268872793, 418.5573905683720568, 3.332260488124728859 ) ) ;
#7262 = CONTEXT_DEPENDENT_SHAPE_REPRESENTATION ( #18552, #11131 ) ;
#7263 = CARTESIAN_POINT ( 'NONE',  ( -11.73070664223724613, 336.0573905765656377, 11.32908994701042005 ) ) ;
#7264 = CARTESIAN_POINT ( 'NONE',  ( 0.000000000000000000, 0.000000000000000000, 0.000000000000000000 ) ) ;
#7265 = CARTESIAN_POINT ( 'NONE',  ( -28.68588794268870856, 316.3698905683720568, 16.75240474999999307 ) ) ;
#7266 = CARTESIAN_POINT ( 'NONE',  ( -42.88789093042844769, 476.3073905683720000, 9.489475012073736337 ) ) ;
#7267 = LINE ( 'NONE', #2207, #3014 ) ;
#7268 = DIRECTION ( 'NONE',  ( -1.000000000000000000, 0.000000000000000000, 0.000000000000000000 ) ) ;
#7269 = CARTESIAN_POINT ( 'NONE',  ( 10.41669750159067220, 172.9933428177121471, 45.00000000000000000 ) ) ;
#7270 = COLOUR_RGB ( '',0.7921568627450980005, 0.8196078431372548767, 0.9333333333333333481 ) ;
#7271 = CARTESIAN_POINT ( 'NONE',  ( -28.68588794268871567, 377.8698905683720000, 16.75240474999999307 ) ) ;
#7272 = VECTOR ( 'NONE', #19893, 1000.000000000000000 ) ;
#7273 = PLANE ( 'NONE',  #15448 ) ;
#7274 = EDGE_CURVE ( 'NONE', #15642, #4181, #11171, .T. ) ;
#7275 = CARTESIAN_POINT ( 'NONE',  ( -48.68588794268872988, 517.2448905601785327, 0.000000000000000000 ) ) ;
#7276 = CARTESIAN_POINT ( 'NONE',  ( -42.88789093042843348, 334.8073905683720000, 9.489475012073736337 ) ) ;
#7277 = ORIENTED_EDGE ( 'NONE', *, *, #7539, .F. ) ;
#7278 = CARTESIAN_POINT ( 'NONE',  ( -25.35362745456399836, 506.6823905683720568, 16.75240474999998952 ) ) ;
#7279 = ORIENTED_EDGE ( 'NONE', *, *, #10583, .F. ) ;
#7280 = AXIS2_PLACEMENT_3D ( 'NONE', #4346, #17539, #2730 ) ;
#7281 = CARTESIAN_POINT ( 'NONE',  ( -47.16347859291444422, 381.3698905765656377, -7.653668647301793193 ) ) ;
#7282 = DIRECTION ( 'NONE',  ( -0.000000000000000000, -0.000000000000000000, -1.000000000000000000 ) ) ;
#7283 = DIRECTION ( 'NONE',  ( 0.000000000000000000, 0.5000000000000018874, 0.8660254037844374864 ) ) ;
#7284 = CARTESIAN_POINT ( 'NONE',  ( -28.68588794268873698, 519.4948905765655809, -19.99999999999999289 ) ) ;
#7285 = CARTESIAN_POINT ( 'NONE',  ( -45.43829269268872650, 473.8698905683720568, 0.000000000000000000 ) ) ;
#7286 = VERTEX_POINT ( 'NONE', #11058 ) ;
#7287 = CARTESIAN_POINT ( 'NONE',  ( -14.48388495494901029, 479.8073905683720568, -9.489475012073734561 ) ) ;
#7288 = CARTESIAN_POINT ( 'NONE',  ( -36.33955658999050087, 249.1198905601784759, 18.47759065022572500 ) ) ;
#7289 = CARTESIAN_POINT ( 'NONE',  ( -45.64106924314019409, 401.0573905765656377, -11.32908994701042715 ) ) ;
#7290 = DIRECTION ( 'NONE',  ( 0.000000000000000000, -0.000000000000000000, -1.000000000000000000 ) ) ;
#7291 = CARTESIAN_POINT ( 'NONE',  ( -32.66413529028186247, 299.4323905601785327, 19.99999999999999289 ) ) ;
#7292 = CARTESIAN_POINT ( 'NONE',  ( -17.35679799567830983, 483.8073905601784190, -16.95518130045146421 ) ) ;
#7293 = CARTESIAN_POINT ( 'NONE',  ( -28.68588794268872633, 484.4948905765656377, 19.99999999999999289 ) ) ;
#7294 = EDGE_CURVE ( 'NONE', #1196, #19472, #17773, .T. ) ;
#7295 = CARTESIAN_POINT ( 'NONE',  ( -8.685887942688532704, 257.3073905765655240, -3.978247347592740013 ) ) ;
#7296 = CARTESIAN_POINT ( 'NONE',  ( -21.03221929538689849, 240.3698905601784759, 18.47759065022572500 ) ) ;
#7297 = FACE_OUTER_BOUND ( 'NONE', #2431, .T. ) ;
#7298 = CARTESIAN_POINT ( 'NONE',  ( -45.43829269268870519, 285.3698905683720568, 0.000000000000000000 ) ) ;
#7299 = CARTESIAN_POINT ( 'NONE',  ( -11.73070664223723192, 251.3073905601784759, 11.32908994701042005 ) ) ;
#7300 = CARTESIAN_POINT ( 'NONE',  ( -48.68588794268898567, 362.3073905765656946, 3.978247347592529071 ) ) ;
#7301 = CARTESIAN_POINT ( 'NONE',  ( -40.53162694259545162, 456.6198905683720568, 11.84573899990672885 ) ) ;
#7302 = CARTESIAN_POINT ( 'NONE',  ( -21.03221929538691981, 328.8698905765656377, -18.47759065022572855 ) ) ;
#7303 = CARTESIAN_POINT ( 'NONE',  ( -19.19641293061497223, 268.8073905683720568, 14.20200298773971426 ) ) ;
#7304 = ORIENTED_EDGE ( 'NONE', *, *, #20266, .F. ) ;
#7305 = VERTEX_POINT ( 'NONE', #9444 ) ;
#7306 = CARTESIAN_POINT ( 'NONE',  ( -44.16309181155858710, 484.7448905683720568, -6.410867750099231266 ) ) ;
#7307 = EDGE_CURVE ( 'NONE', #9225, #11682, #6192, .T. ) ;
#7308 = ORIENTED_EDGE ( 'NONE', *, *, #2400, .T. ) ;
#7309 = CARTESIAN_POINT ( 'NONE',  ( 30.42502041961813575, 271.1055109169419097, -20.00000000000000355 ) ) ;
#7310 = CARTESIAN_POINT ( 'NONE',  ( -19.19641293061496867, 247.3073905683720284, 14.20200298773971426 ) ) ;
#7311 = ORIENTED_EDGE ( 'NONE', *, *, #18119, .T. ) ;
#7312 = CARTESIAN_POINT ( 'NONE',  ( -49.57497958038186425, 230.5765313837437418, -49.99999999999999289 ) ) ;
#7313 = CARTESIAN_POINT ( 'NONE',  ( -28.68588794268872277, 454.4948905765656377, 19.99999999999999289 ) ) ;
#7314 = CARTESIAN_POINT ( 'NONE',  ( 0.2573354458087815932, 4.368923434677187245, 5.432802636760778903 ) ) ;
#7315 = DIRECTION ( 'NONE',  ( 0.000000000000000000, 0.000000000000000000, -1.000000000000000000 ) ) ;
#7316 = CARTESIAN_POINT ( 'NONE',  ( -38.86787825240671168, 223.9102039777116318, -13.30301237467029019 ) ) ;
#7317 = EDGE_CURVE ( 'NONE', #15419, #13742, #9453, .T. ) ;
#7318 = CARTESIAN_POINT ( 'NONE',  ( -19.19641293061499709, 518.8073905683720568, 14.20200298773971426 ) ) ;
#7319 = CYLINDRICAL_SURFACE ( 'NONE', #3524, 5.000000000000001776 ) ;
#7320 = CARTESIAN_POINT ( 'NONE',  ( -28.68588794268870146, 241.3698905683720568, -16.75240474999999307 ) ) ;
#7321 = VECTOR ( 'NONE', #19165, 1000.000000000000114 ) ;
#7322 = CARTESIAN_POINT ( 'NONE',  ( -38.17536295476244845, 336.9323905683720568, 14.20200298773971781 ) ) ;
#7323 = CARTESIAN_POINT ( 'NONE',  ( -14.54375231895776110, 320.9948905601784759, 14.14213562373094568 ) ) ;
#7324 = CARTESIAN_POINT ( 'NONE',  ( -47.16347859291443712, 302.6198905765656377, 7.653668647301805628 ) ) ;
#7325 = CARTESIAN_POINT ( 'NONE',  ( -11.93348319268872615, 398.5573905683720568, 3.332260488124728415 ) ) ;
#7326 = DIRECTION ( 'NONE',  ( 0.000000000000000000, 1.000000000000000000, 0.000000000000000000 ) ) ;
#7327 = CARTESIAN_POINT ( 'NONE',  ( -28.68588794268871922, 384.7448905601785327, -19.99999999999999289 ) ) ;
#7328 = ORIENTED_EDGE ( 'NONE', *, *, #14580, .F. ) ;
#7329 = CARTESIAN_POINT ( 'NONE',  ( -47.16347859291444422, 351.3698905765655809, -7.653668647301793193 ) ) ;
#7330 = ORIENTED_EDGE ( 'NONE', *, *, #4958, .F. ) ;
#7331 = EDGE_LOOP ( 'NONE', ( #6397, #5106, #9467 ) ) ;
#7332 = CARTESIAN_POINT ( 'NONE',  ( -22.27502019258950128, 502.2448905683720568, -15.47720386886985544 ) ) ;
#7333 = CARTESIAN_POINT ( 'NONE',  ( 0.5805565836007606784, -3.752776749732561701, 6.500000000000000000 ) ) ;
#7334 = VERTEX_POINT ( 'NONE', #20095 ) ;
#7335 = CARTESIAN_POINT ( 'NONE',  ( -40.53162694259543031, 306.6198905683720000, 11.84573899990672885 ) ) ;
#7336 = ORIENTED_EDGE ( 'NONE', *, *, #3542, .T. ) ;
#7337 = CARTESIAN_POINT ( 'NONE',  ( -40.53162694259543741, 342.6198905683720000, -11.84573899990672707 ) ) ;
#7338 = CARTESIAN_POINT ( 'NONE',  ( -42.88789093042843348, 344.8073905683719431, 9.489475012073734561 ) ) ;
#7339 = CARTESIAN_POINT ( 'NONE',  ( -17.35679799567828852, 278.5573905765656377, -16.95518130045146421 ) ) ;
#7340 = CARTESIAN_POINT ( 'NONE',  ( -11.73070664223726745, 497.9323905765656377, -11.32908994701042538 ) ) ;
#7341 = CARTESIAN_POINT ( 'NONE',  ( -35.09675569278793006, 241.9948905683720284, -15.47720386886985544 ) ) ;
#7342 = LINE ( 'NONE', #3785, #5296 ) ;
#7343 = EDGE_CURVE ( 'NONE', #11949, #14089, #10144, .T. ) ;
#7344 = CARTESIAN_POINT ( 'NONE',  ( -32.01814843081345430, 407.5573905683720568, 16.75240474999999307 ) ) ;
#7345 = DIRECTION ( 'NONE',  ( 0.000000000000000000, 0.000000000000000000, 1.000000000000000000 ) ) ;
#7346 = CARTESIAN_POINT ( 'NONE',  ( -48.68588794268855935, 451.6823905765656377, -3.978247347593583783 ) ) ;
#7347 =( BOUNDED_CURVE ( )  B_SPLINE_CURVE ( 2, ( #19756, #5258, #16847, #9905, #1597, #18130, #2032, #10012, #10222, #8600, #1822, #6768, #13389, #13283, #11645, #15223, #4940 ),
 .UNSPECIFIED., .F., .T. ) 
 B_SPLINE_CURVE_WITH_KNOTS ( ( 3, 2, 2, 2, 2, 2, 2, 2, 3 ),
 ( 0.1093750000000002914, 0.1113281250000002637, 0.1132812500000002498, 0.1152343750000002220, 0.1171875000000001943, 0.1191406250000001804, 0.1210937500000001527, 0.1230468750000001388, 0.1250000000000001110 ),
 .UNSPECIFIED. ) 
 CURVE ( )  GEOMETRIC_REPRESENTATION_ITEM ( )  RATIONAL_B_SPLINE_CURVE ( ( 0.9999999999999971134, 0.9807852804032333172, 1.000000000000000000, 0.9807852804032304306, 1.000000000000000000, 0.9807852804032304306, 1.000000000000000000, 0.9807852804032304306, 1.000000000000000000, 0.9807852804032304306, 1.000000000000000000, 0.9807852804032304306, 1.000000000000000000, 0.9807852804032304306, 1.000000000000000000, 0.9807852804032293204, 1.000000000000001110 ) ) 
 REPRESENTATION_ITEM ( '' )  );
#7348 = CARTESIAN_POINT ( 'NONE',  ( 60.03793209889851568, 10.52886280891152104, -131.1729372809869005 ) ) ;
#7349 = CARTESIAN_POINT ( 'NONE',  ( -45.43829269268871940, 453.5573905683720568, -3.332260488124726194 ) ) ;
#7350 = ORIENTED_EDGE ( 'NONE', *, *, #7856, .F. ) ;
#7351 = CARTESIAN_POINT ( 'NONE',  ( -28.68588794268872633, 444.7448905601784759, -19.99999999999999289 ) ) ;
#7352 = CARTESIAN_POINT ( 'NONE',  ( -22.27502019258947641, 280.7448905683720568, -15.47720386886985544 ) ) ;
#7353 = ADVANCED_FACE ( 'NONE', ( #7090 ), #3437, .T. ) ;
#7354 = AXIS2_PLACEMENT_3D ( 'NONE', #10420, #9915, #9806 ) ;
#7355 = ORIENTED_EDGE ( 'NONE', *, *, #17106, .T. ) ;
#7356 = EDGE_LOOP ( 'NONE', ( #11946, #18267, #7010, #7837 ) ) ;
#7357 = ORIENTED_EDGE ( 'NONE', *, *, #210, .T. ) ;
#7358 = PLANE ( 'NONE',  #11481 ) ;
#7359 = APPLICATION_CONTEXT ( 'automotive_design' ) ;
#7360 = EDGE_CURVE ( 'NONE', #3989, #17870, #11083, .T. ) ;
#7361 = AXIS2_PLACEMENT_3D ( 'NONE', #7925, #60, #14554 ) ;
#7362 = CARTESIAN_POINT ( 'NONE',  ( -19.19641293061497933, 300.4323905683721136, -14.20200298773971603 ) ) ;
#7363 = EDGE_CURVE ( 'NONE', #11681, #15032, #8399, .T. ) ;
#7364 = CARTESIAN_POINT ( 'NONE',  ( -40.53162694259543741, 366.6198905683720000, 11.84573899990672885 ) ) ;
#7365 = CARTESIAN_POINT ( 'NONE',  ( -32.66413529028186247, 295.0573905601784759, -19.99999999999999289 ) ) ;
#7366 = CARTESIAN_POINT ( 'NONE',  ( -17.35679799567830983, 525.4323905765655809, 16.95518130045146421 ) ) ;
#7367 = CARTESIAN_POINT ( 'NONE',  ( -45.43829269268871940, 403.8698905683720000, 0.000000000000000000 ) ) ;
#7368 = CARTESIAN_POINT ( 'NONE',  ( -32.01814843081343298, 233.1823905683720284, -16.75240474999999307 ) ) ;
#7369 = CARTESIAN_POINT ( 'NONE',  ( -42.88789093042844058, 402.9323905683720568, -9.489475012073734561 ) ) ;
#7370 = CONTEXT_DEPENDENT_SHAPE_REPRESENTATION ( #13325, #21341 ) ;
#7371 = CARTESIAN_POINT ( 'NONE',  ( -8.685887942688720997, 346.9948905765656377, -2.449293598294705724E-15 ) ) ;
#7372 = CARTESIAN_POINT ( 'NONE',  ( -41.83569717483972994, 160.1716627696692683, 25.00000000000000000 ) ) ;
#7373 = CARTESIAN_POINT ( 'NONE',  ( -19.19641293061497223, 297.3073905683720568, 14.20200298773971426 ) ) ;
#7374 =( LENGTH_UNIT ( ) NAMED_UNIT ( * ) SI_UNIT ( .MILLI., .METRE. ) );
#7375 = CARTESIAN_POINT ( 'NONE',  ( -22.27502019258948707, 458.4948905683720568, 15.47720386886985189 ) ) ;
#7376 = EDGE_CURVE ( 'NONE', #15497, #12829, #5163, .T. ) ;
#7377 = CIRCLE ( 'NONE', #6680, 10.00000000000000178 ) ;
#7378 = DIRECTION ( 'NONE',  ( -1.191790137725560488E-16, 1.000000000000000000, -0.000000000000000000 ) ) ;
#7379 = CARTESIAN_POINT ( 'NONE',  ( 4.700000000000000178, 7.505553499465139389, 0.000000000000000000 ) ) ;
#7380 = DIRECTION ( 'NONE',  ( -8.881784197001252323E-16, 0.000000000000000000, 1.000000000000000000 ) ) ;
#7381 = AXIS2_PLACEMENT_3D ( 'NONE', #1708, #11214, #17812 ) ;
#7382 = CARTESIAN_POINT ( 'NONE',  ( -33.77124986504215087, 55.31983858414345434, -120.3516843130412468 ) ) ;
#7383 = CARTESIAN_POINT ( 'NONE',  ( -24.70764059509558308, 534.4323905601785327, -19.99999999999999289 ) ) ;
#7384 = CARTESIAN_POINT ( 'NONE',  ( -35.09675569278794427, 351.9948905683720000, -15.47720386886985544 ) ) ;
#7385 = VERTEX_POINT ( 'NONE', #12073 ) ;
#7386 = CARTESIAN_POINT ( 'NONE',  ( -19.19641293061499709, 507.3073905683720568, 14.20200298773971426 ) ) ;
#7387 = ORIENTED_EDGE ( 'NONE', *, *, #19182, .T. ) ;
#7388 = CARTESIAN_POINT ( 'NONE',  ( -42.82802356641965957, 380.7448905765656377, -14.14213562373094746 ) ) ;
#7389 = LINE ( 'NONE', #2434, #147 ) ;
#7390 = CARTESIAN_POINT ( 'NONE',  ( -165.7253922195053519, 585.7448905601785327, -108.8355377051282034 ) ) ;
#7391 = CARTESIAN_POINT ( 'NONE',  ( -162.2727221670389781, 30.52886280891152282, -4.999999999999990230 ) ) ;
#7392 = CARTESIAN_POINT ( 'NONE',  ( -42.88789093042844769, 454.8073905683720000, 9.489475012073736337 ) ) ;
#7393 = ORIENTED_EDGE ( 'NONE', *, *, #17887, .T. ) ;
#7394 = CARTESIAN_POINT ( 'NONE',  ( -44.16309181155857999, 464.4948905683720000, 6.410867750099241924 ) ) ;
#7395 = DIRECTION ( 'NONE',  ( 1.000000000000000000, 0.000000000000000000, 0.000000000000000000 ) ) ;
#7396 = VECTOR ( 'NONE', #19502, 1000.000000000000000 ) ;
#7397 = CARTESIAN_POINT ( 'NONE',  ( -32.66413529028188378, 409.8073905765656377, -19.99999999999999289 ) ) ;
#7398 = CARTESIAN_POINT ( 'NONE',  ( 51.98438129372387806, -133.1434774248255906, 94.99999999999994316 ) ) ;
#7399 = CARTESIAN_POINT ( 'NONE',  ( -28.68588794268874054, 573.2448905601785327, 0.000000000000000000 ) ) ;
#7400 = DIRECTION ( 'NONE',  ( 0.008660258604321402487, -0.3791853047755957551, -0.9252802302887190855 ) ) ;
#7401 = DIRECTION ( 'NONE',  ( -0.000000000000000000, -0.000000000000000000, 1.000000000000000000 ) ) ;
#7402 = CARTESIAN_POINT ( 'NONE',  ( -36.33955658999049376, 260.1198905765655809, -18.47759065022572855 ) ) ;
#7403 = CARTESIAN_POINT ( 'NONE',  ( -8.685887942688642838, 432.5573905601784759, -3.978247347592952732 ) ) ;
#7404 = CARTESIAN_POINT ( 'NONE',  ( -28.68588794268874054, 588.2448905601785327, 0.000000000000000000 ) ) ;
#7405 = CARTESIAN_POINT ( 'NONE',  ( -22.27502019258947641, 282.2448905683720568, -15.47720386886985544 ) ) ;
#7406 = CARTESIAN_POINT ( 'NONE',  ( -11.73070664223723547, 253.1823905601785043, -11.32908994701042715 ) ) ;
#7407 = FACE_OUTER_BOUND ( 'NONE', #20977, .T. ) ;
#7408 = CARTESIAN_POINT ( 'NONE',  ( -22.27502019258948707, 448.4948905683720568, 15.47720386886985189 ) ) ;
#7409 = CARTESIAN_POINT ( 'NONE',  ( -44.16309181155855867, 264.7448905683720000, -6.410867750099231266 ) ) ;
#7410 = EDGE_LOOP ( 'NONE', ( #769, #14038, #12513, #19574, #1059, #14918 ) ) ;
#7411 = DIRECTION ( 'NONE',  ( -1.191790137725560488E-16, 1.000000000000000000, -0.000000000000000000 ) ) ;
#7412 = EDGE_LOOP ( 'NONE', ( #6565, #1806, #8606, #18909 ) ) ;
#7413 = CARTESIAN_POINT ( 'NONE',  ( -25.35362745456399480, 478.1823905683720568, 16.75240474999998952 ) ) ;
#7414 = EDGE_CURVE ( 'NONE', #15822, #18669, #8411, .T. ) ;
#7415 = ORIENTED_EDGE ( 'NONE', *, *, #11556, .F. ) ;
#7416 = CARTESIAN_POINT ( 'NONE',  ( -8.685887942688742314, 526.9948905765655809, -2.449293598294705724E-15 ) ) ;
#7417 = CARTESIAN_POINT ( 'NONE',  ( -25.35362745456396638, 236.6823905683720284, 16.75240474999998952 ) ) ;
#7418 = ORIENTED_EDGE ( 'NONE', *, *, #14268, .T. ) ;
#7419 = CARTESIAN_POINT ( 'NONE',  ( -28.68588794268874054, 271.1055109169419666, 40.00000000000000000 ) ) ;
#7420 = CARTESIAN_POINT ( 'NONE',  ( -28.68588794268872633, 464.4948905765656377, 19.99999999999999289 ) ) ;
#7421 = CARTESIAN_POINT ( 'NONE',  ( -14.54375231895776999, 390.9948905601784759, 14.14213562373094568 ) ) ;
#7422 = PLANE ( 'NONE',  #9459 ) ;
#7423 = CARTESIAN_POINT ( 'NONE',  ( -28.68588794268870146, 232.8698905683720284, -16.75240474999999307 ) ) ;
#7424 = CARTESIAN_POINT ( 'NONE',  ( -13.20868407381887799, 510.9948905683721136, -6.410867750099233042 ) ) ;
#7425 = LINE ( 'NONE', #5598, #775 ) ;
#7426 = CARTESIAN_POINT ( 'NONE',  ( -35.09675569278793006, 251.9948905683720568, -15.47720386886985544 ) ) ;
#7427 = CARTESIAN_POINT ( 'NONE',  ( -11.93348319268872260, 340.0573905683720000, 3.332260488124728415 ) ) ;
#7428 = ADVANCED_FACE ( 'NONE', ( #3747 ), #10444, .F. ) ;
#7429 = LINE ( 'NONE', #1078, #10571 ) ;
#7430 = CARTESIAN_POINT ( 'NONE',  ( -10.20829729246297823, 306.3698905765655809, 7.653668647301790529 ) ) ;
#7431 = CARTESIAN_POINT ( 'NONE',  ( -25.35362745456399480, 391.0573905683720568, -16.75240474999999307 ) ) ;
#7432 = UNCERTAINTY_MEASURE_WITH_UNIT (LENGTH_MEASURE( 1.000000000000000082E-05 ), #16819, 'distance_accuracy_value', 'NONE');
#7433 = CARTESIAN_POINT ( 'NONE',  ( -18.68588794268873698, 281.1055109169419666, 20.00000000000000355 ) ) ;
#7434 = CARTESIAN_POINT ( 'NONE',  ( -45.64106924314018698, 386.3073905601785327, -11.32908994701042715 ) ) ;
#7435 = EDGE_CURVE ( 'NONE', #4755, #984, #17066, .T. ) ;
#7436 = ORIENTED_EDGE ( 'NONE', *, *, #7586, .F. ) ;
#7437 = CYLINDRICAL_SURFACE ( 'NONE', #21190, 19.99999999999999645 ) ;
#7438 = VERTEX_POINT ( 'NONE', #10131 ) ;
#7439 = ORIENTED_EDGE ( 'NONE', *, *, #12040, .F. ) ;
#7440 = CARTESIAN_POINT ( 'NONE',  ( -40.53162694259545873, 514.1198905683720568, -11.84573899990672707 ) ) ;
#7441 = LINE ( 'NONE', #14067, #20789 ) ;
#7442 = ORIENTED_EDGE ( 'NONE', *, *, #20909, .T. ) ;
#7443 = CARTESIAN_POINT ( 'NONE',  ( -13.20868407381885312, 300.9948905683720568, -6.410867750099233042 ) ) ;
#7444 = ORIENTED_EDGE ( 'NONE', *, *, #635, .F. ) ;
#7445 = CARTESIAN_POINT ( 'NONE',  ( -40.53162694259543741, 335.1198905683720568, 11.84573899990672885 ) ) ;
#7446 = CARTESIAN_POINT ( 'NONE',  ( -40.53162694259543741, 352.6198905683720000, -11.84573899990672707 ) ) ;
#7447 = CARTESIAN_POINT ( 'NONE',  ( -42.82802356641965247, 293.2448905765655809, 14.14213562373094923 ) ) ;
#7448 = LINE ( 'NONE', #4222, #18282 ) ;
#7449 = CARTESIAN_POINT ( 'NONE',  ( -14.48388495494898365, 237.9323905683720000, 9.489475012073731008 ) ) ;
#7450 = CARTESIAN_POINT ( 'NONE',  ( -42.82802356641963826, 204.8142847187655491, 5.000000000000000000 ) ) ;
#7451 = CARTESIAN_POINT ( 'NONE',  ( -38.17536295476246266, 393.8073905683720000, -14.20200298773971426 ) ) ;
#7452 = EDGE_CURVE ( 'NONE', #19877, #13421, #11662, .T. ) ;
#7453 = FACE_OUTER_BOUND ( 'NONE', #13376, .T. ) ;
#7454 = DIRECTION ( 'NONE',  ( 0.000000000000000000, 0.8660254037844375974, -0.5000000000000018874 ) ) ;
#7455 = LINE ( 'NONE', #6154, #3562 ) ;
#7456 = CARTESIAN_POINT ( 'NONE',  ( -19.19641293061498999, 437.3073905683720000, 14.20200298773971426 ) ) ;
#7457 = ORIENTED_EDGE ( 'NONE', *, *, #11510, .T. ) ;
#7458 = CARTESIAN_POINT ( 'NONE',  ( -14.54375231895777532, 440.9948905601784759, 14.14213562373094568 ) ) ;
#7459 = EDGE_LOOP ( 'NONE', ( #16832, #17796, #21363, #2724 ) ) ;
#7460 = CARTESIAN_POINT ( 'NONE',  ( 5.299999999999999822, 3.752776749732563033, 6.500000000000000000 ) ) ;
#7461 = ORIENTED_EDGE ( 'NONE', *, *, #16181, .F. ) ;
#7462 = ORIENTED_EDGE ( 'NONE', *, *, #21349, .T. ) ;
#7463 = CARTESIAN_POINT ( 'NONE',  ( 0.000000000000000000, 7.511572993685794170E-16, -6.499999999999999112 ) ) ;
#7464 = CARTESIAN_POINT ( 'NONE',  ( -40.01497788969912506, 318.8073905601784759, 16.95518130045146776 ) ) ;
#7465 = CARTESIAN_POINT ( 'NONE',  ( -11.93348319268871727, 308.5573905683719431, 3.332260488124728415 ) ) ;
#7466 = CARTESIAN_POINT ( 'NONE',  ( -22.27502019258947641, 368.4948905683720568, 15.47720386886985189 ) ) ;
#7467 = AXIS2_PLACEMENT_3D ( 'NONE', #3302, #9875, #13031 ) ;
#7468 = DIRECTION ( 'NONE',  ( 0.000000000000000000, 0.000000000000000000, 1.000000000000000000 ) ) ;
#7469 = CARTESIAN_POINT ( 'NONE',  ( -14.54375231895779130, 528.2448905765656946, -14.14213562373094746 ) ) ;
#7470 = CARTESIAN_POINT ( 'NONE',  ( -32.01814843081345430, 406.0573905683720000, 16.75240474999999307 ) ) ;
#7471 = CARTESIAN_POINT ( 'NONE',  ( -11.93348319268870839, 250.6823905683720852, -3.332260488124732856 ) ) ;
#7472 = CARTESIAN_POINT ( 'NONE',  ( -28.68588794268872277, 411.3698905683720568, -16.75240474999999307 ) ) ;
#7473 = CARTESIAN_POINT ( 'NONE',  ( -42.82802356641965957, 350.7448905765655809, -14.14213562373094746 ) ) ;
#7474 = CARTESIAN_POINT ( 'NONE',  ( -24.70764059509555466, 324.4323905601784190, -19.99999999999999289 ) ) ;
#7475 = CARTESIAN_POINT ( 'NONE',  ( -32.01814843081344009, 301.6823905683720568, -16.75240474999999307 ) ) ;
#7476 = DIRECTION ( 'NONE',  ( 0.000000000000000000, 0.000000000000000000, 1.000000000000000000 ) ) ;
#7477 = CARTESIAN_POINT ( 'NONE',  ( -44.16309181155857999, 465.9948905683720000, 6.410867750099241924 ) ) ;
#7478 = CARTESIAN_POINT ( 'NONE',  ( 10.41669750159067220, 172.9933428177121471, 45.00000000000000000 ) ) ;
#7479 = PLANE ( 'NONE',  #3153 ) ;
#7480 = CARTESIAN_POINT ( 'NONE',  ( 163.6892970195449948, 191.6575133381268756, -49.76543245040357277 ) ) ;
#7481 = EDGE_CURVE ( 'NONE', #7137, #14447, #20730, .T. ) ;
#7482 = VECTOR ( 'NONE', #9007, 1000.000000000000000 ) ;
#7483 = CARTESIAN_POINT ( 'NONE',  ( -25.35362745456399125, 362.5573905683720568, -16.75240474999999307 ) ) ;
#7484 = CARTESIAN_POINT ( 'NONE',  ( -8.685887942688719221, 332.2448905601784759, -2.449293598294705724E-15 ) ) ;
#7485 = APPLICATION_CONTEXT ( 'automotive_design' ) ;
#7486 = CARTESIAN_POINT ( 'NONE',  ( -10.20829729246300310, 512.8698905601785327, -7.653668647301794969 ) ) ;
#7487 = CARTESIAN_POINT ( 'NONE',  ( -28.68588794268871212, 341.3698905683720000, -16.75240474999999307 ) ) ;
#7488 = CIRCLE ( 'NONE', #10248, 4.999999999999990230 ) ;
#7489 = VERTEX_POINT ( 'NONE', #12400 ) ;
#7490 = CARTESIAN_POINT ( 'NONE',  ( -16.84014894278200458, 507.6198905683720000, 11.84573899990672530 ) ) ;
#7491 = PRODUCT ( 'hex screw gradeab_iso_ISO 4017 - M8 x 16-N', 'hex screw gradeab_iso_ISO 4017 - M8 x 16-N', '', ( #15190 ) ) ;
#7492 = VERTEX_POINT ( 'NONE', #9143 ) ;
#7493 = CARTESIAN_POINT ( 'NONE',  ( 164.2593879927715932, 166.6963511708817691, 60.00000000000000000 ) ) ;
#7494 = EDGE_CURVE ( 'NONE', #13587, #18118, #2131, .T. ) ;
#7495 = CARTESIAN_POINT ( 'NONE',  ( -44.16309181155857999, 414.7448905683720568, -6.410867750099231266 ) ) ;
#7496 = DIRECTION ( 'NONE',  ( 9.855701800883827197E-17, -1.000000000000000000, 9.855701800883827197E-17 ) ) ;
#7497 = CYLINDRICAL_SURFACE ( 'NONE', #6577, 40.00000000000000000 ) ;
#7498 = CARTESIAN_POINT ( 'NONE',  ( -22.27502019258949773, 460.7448905683720568, -15.47720386886985544 ) ) ;
#7499 = ORIENTED_EDGE ( 'NONE', *, *, #6491, .F. ) ;
#7500 = CARTESIAN_POINT ( 'NONE',  ( -16.84014894278200103, 467.6198905683720000, 11.84573899990672530 ) ) ;
#7501 = CARTESIAN_POINT ( 'NONE',  ( 69.55160839065807465, 152.8169032537915086, 64.80145223029053625 ) ) ;
#7502 = AXIS2_PLACEMENT_3D ( 'NONE', #7399, #2765, #12500 ) ;
#7503 = CARTESIAN_POINT ( 'NONE',  ( -32.66413529028188378, 404.1823905765656946, 19.99999999999999289 ) ) ;
#7504 = CARTESIAN_POINT ( 'NONE',  ( -8.685887942688742314, 573.2448905601785327, 2.449293598294706119E-15 ) ) ;
#7505 = CARTESIAN_POINT ( 'NONE',  ( -14.54375231895777176, 368.2448905765656377, -14.14213562373094746 ) ) ;
#7506 = CARTESIAN_POINT ( 'NONE',  ( 163.6892970195449948, 191.6575133381268756, 49.76543245040357277 ) ) ;
#7507 = DIRECTION ( 'NONE',  ( 0.000000000000000000, 0.000000000000000000, 1.000000000000000000 ) ) ;
#7508 = VECTOR ( 'NONE', #1624, 1000.000000000000000 ) ;
#7509 = DIRECTION ( 'NONE',  ( 0.000000000000000000, 1.000000000000000000, -0.000000000000000000 ) ) ;
#7510 = CARTESIAN_POINT ( 'NONE',  ( -48.68588794268878672, 237.5573905601784475, 3.978247347592954952 ) ) ;
#7511 = LINE ( 'NONE', #9462, #4179 ) ;
#7512 = CARTESIAN_POINT ( 'NONE',  ( -44.16309181155855867, 275.9948905683720000, 6.410867750099241924 ) ) ;
#7513 = CARTESIAN_POINT ( 'NONE',  ( -24.70764059509554755, 244.4323905601784759, -19.99999999999999289 ) ) ;
#7514 = CARTESIAN_POINT ( 'NONE',  ( -24.70764059509554755, 364.8073905765656377, 19.99999999999998934 ) ) ;
#7515 = CARTESIAN_POINT ( 'NONE',  ( -22.27502019258948351, 428.4948905683720568, 15.47720386886985189 ) ) ;
#7516 = CARTESIAN_POINT ( 'NONE',  ( -28.68588794268871922, 399.4948905765656377, -19.99999999999999289 ) ) ;
#7517 = CARTESIAN_POINT ( 'NONE',  ( -44.16309181155855157, 245.9948905683720284, 6.410867750099241924 ) ) ;
#7518 = ORIENTED_EDGE ( 'NONE', *, *, #3500, .F. ) ;
#7519 = CARTESIAN_POINT ( 'NONE',  ( -8.685887942688742314, 573.2448905601785327, 2.449293598294706119E-15 ) ) ;
#7520 = ORIENTED_EDGE ( 'NONE', *, *, #401, .F. ) ;
#7521 = CARTESIAN_POINT ( 'NONE',  ( -42.88789093042844769, 484.4323905683720000, -9.489475012073734561 ) ) ;
#7522 = ORIENTED_EDGE ( 'NONE', *, *, #10059, .F. ) ;
#7523 = LINE ( 'NONE', #4294, #1756 ) ;
#7524 = CARTESIAN_POINT ( 'NONE',  ( -32.01814843081343298, 241.6823905683720568, -16.75240474999999307 ) ) ;
#7525 = ORIENTED_EDGE ( 'NONE', *, *, #115, .T. ) ;
#7526 = CARTESIAN_POINT ( 'NONE',  ( -25.35362745456401257, 521.0573905683719431, -16.75240474999999307 ) ) ;
#7527 = DIRECTION ( 'NONE',  ( -1.000000000000000000, 0.000000000000000000, 0.000000000000000000 ) ) ;
#7528 = CARTESIAN_POINT ( 'NONE',  ( -47.16347859291445843, 462.6198905765655809, 7.653668647301805628 ) ) ;
#7529 = CARTESIAN_POINT ( 'NONE',  ( -14.54375231895776466, 350.9948905601784759, 14.14213562373094568 ) ) ;
#7530 = CYLINDRICAL_SURFACE ( 'NONE', #2878, 19.99999999999999645 ) ;
#7531 = CARTESIAN_POINT ( 'NONE',  ( -31.59713164724962198, 223.9102039777117454, -17.88048509134786812 ) ) ;
#7532 = CARTESIAN_POINT ( 'NONE',  ( 78.68120802659203150, 149.7457237375499517, -66.14548919766382085 ) ) ;
#7533 = CARTESIAN_POINT ( 'NONE',  ( -22.27502019258949417, 508.4948905683720568, 15.47720386886985189 ) ) ;
#7534 = CARTESIAN_POINT ( 'NONE',  ( 0.5805565836007647862, 7.505553499465139389, 2.227827669841787811E-16 ) ) ;
#7535 = CARTESIAN_POINT ( 'NONE',  ( -22.27502019258946220, 256.9948905683720568, 15.47720386886985189 ) ) ;
#7536 = CARTESIAN_POINT ( 'NONE',  ( -45.43829269268870519, 335.0573905683720568, -3.332260488124726194 ) ) ;
#7537 = CARTESIAN_POINT ( 'NONE',  ( -47.16347859291445843, 467.8698905601784759, 7.653668647301805628 ) ) ;
#7538 = CARTESIAN_POINT ( 'NONE',  ( -32.66413529028186247, 304.1823905765655809, 19.99999999999999289 ) ) ;
#7539 = EDGE_CURVE ( 'NONE', #6352, #16482, #953, .T. ) ;
#7540 = CARTESIAN_POINT ( 'NONE',  ( -28.68588794268871567, 386.3698905683720568, 16.75240474999999307 ) ) ;
#7541 = ADVANCED_FACE ( 'NONE', ( #2667 ), #12294, .T. ) ;
#7542 = CARTESIAN_POINT ( 'NONE',  ( -8.685887942688728103, 422.2448905601784759, -2.449293598294705724E-15 ) ) ;
#7543 = CARTESIAN_POINT ( 'NONE',  ( -47.16347859291444422, 377.8698905601784190, 7.653668647301805628 ) ) ;
#7544 = CIRCLE ( 'NONE', #8583, 15.00000000000000355 ) ;
#7545 = ORIENTED_EDGE ( 'NONE', *, *, #15811, .T. ) ;
#7546 = DIRECTION ( 'NONE',  ( -0.3717199501173604759, 0.000000000000000000, 0.9283449136418786551 ) ) ;
#7547 = ORIENTED_EDGE ( 'NONE', *, *, #16367, .F. ) ;
#7548 = ORIENTED_EDGE ( 'NONE', *, *, #20195, .T. ) ;
#7549 = CARTESIAN_POINT ( 'NONE',  ( -25.35362745456399836, 498.1823905683720000, 16.75240474999998952 ) ) ;
#7550 = CARTESIAN_POINT ( 'NONE',  ( -8.685887942688980345, 296.6823905765654104, 3.978247347593800054 ) ) ;
#7551 = VERTEX_POINT ( 'NONE', #14144 ) ;
#7552 = CARTESIAN_POINT ( 'NONE',  ( -22.27502019258947996, 312.2448905683720000, -15.47720386886985544 ) ) ;
#7553 = EDGE_LOOP ( 'NONE', ( #19047, #7782, #13593, #8296, #14811, #2484 ) ) ;
#7554 = CARTESIAN_POINT ( 'NONE',  ( -14.48388495494899431, 327.9323905683720568, 9.489475012073732785 ) ) ;
#7555 = CARTESIAN_POINT ( 'NONE',  ( -44.16309181155856578, 344.4948905683720000, 6.410867750099241924 ) ) ;
#7556 = CARTESIAN_POINT ( 'NONE',  ( -40.01497788969912506, 293.5573905765656377, 16.95518130045146776 ) ) ;
#7557 = CARTESIAN_POINT ( 'NONE',  ( -28.68588794268872633, 250.8848358243226357, 40.00000000000000000 ) ) ;
#7558 = CARTESIAN_POINT ( 'NONE',  ( -42.88789093042841927, 244.8073905683720568, 9.489475012073734561 ) ) ;
#7559 = CARTESIAN_POINT ( 'NONE',  ( -19.19641293061498999, 401.9323905683720000, -14.20200298773971603 ) ) ;
#7560 = AXIS2_PLACEMENT_3D ( 'NONE', #8916, #15537, #7290 ) ;
#7561 = EDGE_CURVE ( 'NONE', #1608, #3040, #15660, .T. ) ;
#7562 = CARTESIAN_POINT ( 'NONE',  ( 116.0391604516428430, 192.9550247130592027, 40.00000000000000000 ) ) ;
#7563 = CARTESIAN_POINT ( 'NONE',  ( 5.674999999999999822, 7.960204194457796463E-16, -6.500000000000000888 ) ) ;
#7564 = CARTESIAN_POINT ( 'NONE',  ( -10.20829729246297291, 242.8698905601785043, -7.653668647301794969 ) ) ;
#7565 = CARTESIAN_POINT ( 'NONE',  ( -42.88789093042844769, 452.9323905683720568, -9.489475012073736337 ) ) ;
#7566 = EDGE_LOOP ( 'NONE', ( #1093, #15920, #4889 ) ) ;
#7567 = CARTESIAN_POINT ( 'NONE',  ( -48.68588794268871567, 437.2448905601785327, 0.000000000000000000 ) ) ;
#7568 = ORIENTED_EDGE ( 'NONE', *, *, #2723, .F. ) ;
#7569 = DIRECTION ( 'NONE',  ( 9.855701800883827197E-17, -1.000000000000000000, 9.855701800883827197E-17 ) ) ;
#7570 = EDGE_LOOP ( 'NONE', ( #14966, #6266, #2508 ) ) ;
#7571 = ORIENTED_EDGE ( 'NONE', *, *, #17240, .T. ) ;
#7572 = DIRECTION ( 'NONE',  ( -0.000000000000000000, -1.000000000000000000, -0.000000000000000000 ) ) ;
#7573 = CARTESIAN_POINT ( 'NONE',  ( -48.68588794268870146, 327.2448905601785327, 0.000000000000000000 ) ) ;
#7574 = AXIS2_PLACEMENT_3D ( 'NONE', #17521, #15698, #5941 ) ;
#7575 = EDGE_CURVE ( 'NONE', #15608, #19602, #846, .T. ) ;
#7576 = CARTESIAN_POINT ( 'NONE',  ( -11.93348319268872260, 370.6823905683719431, -3.332260488124732856 ) ) ;
#7577 = DIRECTION ( 'NONE',  ( -1.191790137725560488E-16, 1.000000000000000000, -0.000000000000000000 ) ) ;
#7578 = CARTESIAN_POINT ( 'NONE',  ( -32.66413529028189799, 524.1823905765656946, 19.99999999999999289 ) ) ;
#7579 = CARTESIAN_POINT ( 'NONE',  ( -13.20868407381886378, 408.2448905683720568, 6.410867750099229490 ) ) ;
#7580 = CARTESIAN_POINT ( 'NONE',  ( -44.16309181155855867, 234.7448905683720000, -6.410867750099231266 ) ) ;
#7581 = CARTESIAN_POINT ( 'NONE',  ( -25.35362745456398770, 406.6823905683719431, 16.75240474999998952 ) ) ;
#7582 = CARTESIAN_POINT ( 'NONE',  ( -36.33955658999050797, 350.1198905765656377, -18.47759065022572855 ) ) ;
#7583 = DIRECTION ( 'NONE',  ( -1.000000000000000000, 0.000000000000000000, 0.000000000000000000 ) ) ;
#7584 = CARTESIAN_POINT ( 'NONE',  ( -32.01814843081344009, 306.0573905683720000, 16.75240474999999307 ) ) ;
#7585 = CARTESIAN_POINT ( 'NONE',  ( -22.27502019258949773, 452.2448905683720000, -15.47720386886985544 ) ) ;
#7586 = EDGE_CURVE ( 'NONE', #19261, #17559, #20619, .T. ) ;
#7587 = DIRECTION ( 'NONE',  ( 0.000000000000000000, -1.000000000000000000, 0.000000000000000000 ) ) ;
#7588 = DIRECTION ( 'NONE',  ( 1.191790137725560488E-16, -1.000000000000000000, -0.000000000000000000 ) ) ;
#7589 = CARTESIAN_POINT ( 'NONE',  ( 3.458603197740078627, 160.1716627696692683, 33.59072564020503648 ) ) ;
#7590 = CARTESIAN_POINT ( 'NONE',  ( -38.17536295476244845, 376.9323905683719431, 14.20200298773971781 ) ) ;
#7591 = CARTESIAN_POINT ( 'NONE',  ( -13.20868407381887799, 509.4948905683720568, -6.410867750099233042 ) ) ;
#7592 = CARTESIAN_POINT ( 'NONE',  ( -14.54375231895778420, 510.9948905601784190, 14.14213562373094568 ) ) ;
#7593 = CARTESIAN_POINT ( 'NONE',  ( -35.09675569278793716, 321.9948905683720568, -15.47720386886985544 ) ) ;
#7594 = ORIENTED_EDGE ( 'NONE', *, *, #12639, .F. ) ;
#7595 = CARTESIAN_POINT ( 'NONE',  ( -38.17536295476246977, 502.3073905683720568, -14.20200298773971426 ) ) ;
#7596 = ORIENTED_EDGE ( 'NONE', *, *, #20720, .F. ) ;
#7597 = CARTESIAN_POINT ( 'NONE',  ( -48.68588794268872277, 457.2448905601784759, 0.000000000000000000 ) ) ;
#7598 = CARTESIAN_POINT ( 'NONE',  ( -13.20868407381886733, 420.9948905683720000, -6.410867750099233042 ) ) ;
#7599 = CARTESIAN_POINT ( 'NONE',  ( -40.01497788969911795, 233.5573905765656093, 16.95518130045146776 ) ) ;
#7600 = CARTESIAN_POINT ( 'NONE',  ( -14.54375231895778953, 518.2448905765656946, -14.14213562373094746 ) ) ;
#7601 = CARTESIAN_POINT ( 'NONE',  ( -38.17536295476246977, 462.3073905683720568, -14.20200298773971426 ) ) ;
#7602 = ORIENTED_EDGE ( 'NONE', *, *, #12926, .F. ) ;
#7603 = CARTESIAN_POINT ( 'NONE',  ( -14.48388495494901029, 457.9323905683720000, 9.489475012073731008 ) ) ;
#7604 =( BOUNDED_CURVE ( )  B_SPLINE_CURVE ( 2, ( #12707, #4790, #16386, #8132, #12813, #17569, #2868, #21348, #17781, #9451, #6092, #3073, #16068, #11386, #19509, #20925, #6516 ),
 .UNSPECIFIED., .F., .T. ) 
 B_SPLINE_CURVE_WITH_KNOTS ( ( 3, 2, 2, 2, 2, 2, 2, 2, 3 ),
 ( 0.3750000000000001665, 0.3769531250000001665, 0.3789062500000001665, 0.3808593750000001665, 0.3828125000000001665, 0.3847656250000001665, 0.3867187500000001665, 0.3886718750000001665, 0.3906250000000001665 ),
 .UNSPECIFIED. ) 
 CURVE ( )  GEOMETRIC_REPRESENTATION_ITEM ( )  RATIONAL_B_SPLINE_CURVE ( ( 0.9999999999999983347, 0.9807852804032320959, 1.000000000000000000, 0.9807852804032304306, 1.000000000000000000, 0.9807852804032304306, 1.000000000000000000, 0.9807852804032304306, 1.000000000000000000, 0.9807852804032304306, 1.000000000000000000, 0.9807852804032304306, 1.000000000000000000, 0.9807852804032304306, 1.000000000000000000, 0.9807852804032287652, 1.000000000000001554 ) ) 
 REPRESENTATION_ITEM ( '' )  );
#7605 = CARTESIAN_POINT ( 'NONE',  ( -4.001383642829314802E-15, 5.309483803148796532, 3.803704290982252267 ) ) ;
#7606 = AXIS2_PLACEMENT_3D ( 'NONE', #9338, #1454, #19612 ) ;
#7607 = CARTESIAN_POINT ( 'NONE',  ( -32.66413529028188378, 394.1823905765655809, 19.99999999999999289 ) ) ;
#7608 = CARTESIAN_POINT ( 'NONE',  ( -28.68588794268870501, 279.4948905765656377, -19.99999999999999289 ) ) ;
#7609 = FACE_OUTER_BOUND ( 'NONE', #3251, .T. ) ;
#7610 = CARTESIAN_POINT ( 'NONE',  ( 0.000000000000000000, 5.629165124598846326, -3.250000000000007550 ) ) ;
#7611 = CARTESIAN_POINT ( 'NONE',  ( -14.54375231895778242, 485.7448905765656377, 14.14213562373094568 ) ) ;
#7612 = VECTOR ( 'NONE', #12054, 1000.000000000000114 ) ;
#7613 = DIRECTION ( 'NONE',  ( 0.000000000000000000, -0.5000000000000011102, -0.8660254037844379305 ) ) ;
#7614 = VECTOR ( 'NONE', #9639, 1000.000000000000114 ) ;
#7615 = CARTESIAN_POINT ( 'NONE',  ( -36.33955658999049376, 255.3698905601785043, -18.47759065022572855 ) ) ;
#7616 = CARTESIAN_POINT ( 'NONE',  ( -43.03936164446626833, 223.9102039777117454, 11.81008090239473773 ) ) ;
#7617 = ADVANCED_FACE ( 'NONE', ( #10765, #19211 ), #1061, .F. ) ;
#7618 = EDGE_CURVE ( 'NONE', #11300, #17480, #10647, .T. ) ;
#7619 = CARTESIAN_POINT ( 'NONE',  ( -32.66413529028186247, 255.0573905601785043, -19.99999999999999289 ) ) ;
#7620 = CARTESIAN_POINT ( 'NONE',  ( -17.35679799567828852, 365.4323905765656377, 16.95518130045146421 ) ) ;
#7621 = CARTESIAN_POINT ( 'NONE',  ( -42.88789093042844058, 434.4323905683720568, -9.489475012073736337 ) ) ;
#7622 = CARTESIAN_POINT ( 'NONE',  ( -11.73070664223723547, 266.0573905765656377, 11.32908994701042005 ) ) ;
#7623 = AXIS2_PLACEMENT_3D ( 'NONE', #12522, #4298, #15880 ) ;
#7624 = CARTESIAN_POINT ( 'NONE',  ( -45.43829269268869808, 245.3698905683720568, 0.000000000000000000 ) ) ;
#7625 = ORIENTED_EDGE ( 'NONE', *, *, #9827, .F. ) ;
#7626 = ORIENTED_EDGE ( 'NONE', *, *, #2898, .F. ) ;
#7627 = CARTESIAN_POINT ( 'NONE',  ( -28.68588794268869790, 223.9102039777116602, 0.000000000000000000 ) ) ;
#7628 = ORIENTED_EDGE ( 'NONE', *, *, #9300, .T. ) ;
#7629 = CARTESIAN_POINT ( 'NONE',  ( -42.88789093042844769, 464.4323905683720000, -9.489475012073734561 ) ) ;
#7630 = EDGE_CURVE ( 'NONE', #15821, #15878, #20511, .T. ) ;
#7631 = AXIS2_PLACEMENT_3D ( 'NONE', #6342, #21171, #4723 ) ;
#7632 = VECTOR ( 'NONE', #3925, 1000.000000000000000 ) ;
#7633 = VERTEX_POINT ( 'NONE', #20942 ) ;
#7634 = CARTESIAN_POINT ( 'NONE',  ( -48.68588794268870856, 367.2448905601784759, 0.000000000000000000 ) ) ;
#7635 = CARTESIAN_POINT ( 'NONE',  ( -22.27502019258946220, 246.9948905683720284, 15.47720386886985189 ) ) ;
#7636 = VERTEX_POINT ( 'NONE', #11402 ) ;
#7637 = CARTESIAN_POINT ( 'NONE',  ( -14.48388495494901562, 517.9323905683720568, 9.489475012073731008 ) ) ;
#7638 = CARTESIAN_POINT ( 'NONE',  ( 151.4788465195079823, 610.7448905601785327, -8.917803138848077182 ) ) ;
#7639 = EDGE_CURVE ( 'NONE', #4929, #17485, #11196, .T. ) ;
#7640 = CARTESIAN_POINT ( 'NONE',  ( -24.70764059509556532, 464.8073905765656377, 19.99999999999998934 ) ) ;
#7641 = CARTESIAN_POINT ( 'NONE',  ( 0.000000000000000000, -5.629165124598843661, 3.250000000000012879 ) ) ;
#7642 = CARTESIAN_POINT ( 'NONE',  ( -45.64106924314017277, 282.9323905765656377, 11.32908994701042538 ) ) ;
#7643 = FACE_BOUND ( 'NONE', #3906, .T. ) ;
#7644 = ADVANCED_BREP_SHAPE_REPRESENTATION ( '', ( #11152, #12794 ), #32 ) ;
#7645 = CARTESIAN_POINT ( 'NONE',  ( -28.68588794268869435, 227.8698905683720284, 16.75240474999999307 ) ) ;
#7646 = CARTESIAN_POINT ( 'NONE',  ( -8.685887942688735208, 466.9948905765656377, -2.449293598294705724E-15 ) ) ;
#7647 = CARTESIAN_POINT ( 'NONE',  ( -35.09675569278793006, 221.9948905683720284, -15.47720386886985544 ) ) ;
#7648 = CARTESIAN_POINT ( 'NONE',  ( -38.17536295476245556, 343.8073905683720000, -14.20200298773971426 ) ) ;
#7649 = EDGE_CURVE ( 'NONE', #18462, #6752, #1340, .T. ) ;
#7650 = CARTESIAN_POINT ( 'NONE',  ( -36.33955658999050797, 319.1198905601784759, 18.47759065022572500 ) ) ;
#7651 = CARTESIAN_POINT ( 'NONE',  ( 0.000000000000000000, 0.000000000000000000, 6.500000000000000000 ) ) ;
#7652 = CARTESIAN_POINT ( 'NONE',  ( -38.17536295476244135, 316.9323905683719431, 14.20200298773971781 ) ) ;
#7653 = CARTESIAN_POINT ( 'NONE',  ( -32.01814843081344719, 376.0573905683720000, 16.75240474999999307 ) ) ;
#7654 = CARTESIAN_POINT ( 'NONE',  ( -18.68588794268873698, 281.1055109169419666, 40.00000000000000000 ) ) ;
#7655 = CARTESIAN_POINT ( 'NONE',  ( -14.54375231895777354, 393.4948905601784190, -14.14213562373094746 ) ) ;
#7656 = CARTESIAN_POINT ( 'NONE',  ( 29.72350413846044859, 280.4463447002762564, 40.00000000000000000 ) ) ;
#7657 = EDGE_LOOP ( 'NONE', ( #5080, #13093, #3961, #3253 ) ) ;
#7658 = VERTEX_POINT ( 'NONE', #17692 ) ;
#7659 = CARTESIAN_POINT ( 'NONE',  ( -45.43829269268871940, 505.0573905683721136, -3.332260488124726194 ) ) ;
#7660 = FACE_OUTER_BOUND ( 'NONE', #12569, .T. ) ;
#7661 = ORIENTED_EDGE ( 'NONE', *, *, #17122, .T. ) ;
#7662 = CARTESIAN_POINT ( 'NONE',  ( -38.17536295476244845, 303.8073905683720000, -14.20200298773971426 ) ) ;
#7663 = ORIENTED_EDGE ( 'NONE', *, *, #5129, .F. ) ;
#7664 = CARTESIAN_POINT ( 'NONE',  ( -42.88789093042843348, 332.9323905683720568, -9.489475012073736337 ) ) ;
#7665 = VECTOR ( 'NONE', #17468, 1000.000000000000000 ) ;
#7666 = CARTESIAN_POINT ( 'NONE',  ( -17.35679799567828141, 265.4323905765656377, 16.95518130045146421 ) ) ;
#7667 = CARTESIAN_POINT ( 'NONE',  ( -8.685887942688742314, 573.2448905601785327, 2.449293598294706119E-15 ) ) ;
#7668 = ADVANCED_FACE ( 'NONE', ( #18005 ), #3199, .T. ) ;
#7669 = CARTESIAN_POINT ( 'NONE',  ( -40.53162694259542320, 242.6198905683720284, -11.84573899990672707 ) ) ;
#7670 = CYLINDRICAL_SURFACE ( 'NONE', #19821, 19.99999999999999645 ) ;
#7671 =( BOUNDED_CURVE ( )  B_SPLINE_CURVE ( 2, ( #19014, #18901, #20861, #4198, #10673, #9274, #10784, #19128, #974, #17606, #2369, #5812, #12420, #5704, #7537, #20750, #14276 ),
 .UNSPECIFIED., .F., .T. ) 
 B_SPLINE_CURVE_WITH_KNOTS ( ( 3, 2, 2, 2, 2, 2, 2, 2, 3 ),
 ( 0.2031250000000001665, 0.2050781250000001665, 0.2070312500000001665, 0.2089843750000001665, 0.2109375000000001665, 0.2128906250000001943, 0.2148437500000001943, 0.2167968750000001943, 0.2187500000000001943 ),
 .UNSPECIFIED. ) 
 CURVE ( )  GEOMETRIC_REPRESENTATION_ITEM ( )  RATIONAL_B_SPLINE_CURVE ( ( 0.9999999999999983347, 0.9807852804032320959, 1.000000000000000000, 0.9807852804032304306, 1.000000000000000000, 0.9807852804032304306, 1.000000000000000000, 0.9807852804032304306, 1.000000000000000000, 0.9807852804032304306, 1.000000000000000000, 0.9807852804032304306, 1.000000000000000000, 0.9807852804032304306, 1.000000000000000000, 0.9807852804032285432, 1.000000000000001998 ) ) 
 REPRESENTATION_ITEM ( '' )  );
#7672 = CARTESIAN_POINT ( 'NONE',  ( -35.09675569278795848, 407.2448905683720568, 15.47720386886985366 ) ) ;
#7673 = DIRECTION ( 'NONE',  ( 0.000000000000000000, 0.000000000000000000, -1.000000000000000000 ) ) ;
#7674 = CARTESIAN_POINT ( 'NONE',  ( 30.42502041961813575, 271.1055109169419097, 40.00000000000000000 ) ) ;
#7675 = AXIS2_PLACEMENT_3D ( 'NONE', #19973, #197, #1707 ) ;
#7676 = CARTESIAN_POINT ( 'NONE',  ( -36.33955658999049376, 245.3698905601785043, -18.47759065022572855 ) ) ;
#7677 = CARTESIAN_POINT ( 'NONE',  ( -28.68588794268872277, 436.3698905683720000, 16.75240474999999307 ) ) ;
#7678 = ORIENTED_EDGE ( 'NONE', *, *, #19607, .T. ) ;
#7679 = CARTESIAN_POINT ( 'NONE',  ( -8.685887942688731655, 452.5573905601784759, -3.978247347593165895 ) ) ;
#7680 = ORIENTED_EDGE ( 'NONE', *, *, #3878, .T. ) ;
#7681 = ORIENTED_EDGE ( 'NONE', *, *, #13784, .F. ) ;
#7682 = ORIENTED_EDGE ( 'NONE', *, *, #8792, .F. ) ;
#7683 = DIRECTION ( 'NONE',  ( 0.000000000000000000, 0.000000000000000000, -1.000000000000000000 ) ) ;
#7684 = CARTESIAN_POINT ( 'NONE',  ( -8.685887942688719221, 332.2448905601784759, -2.449293598294705724E-15 ) ) ;
#7685 = ADVANCED_FACE ( 'NONE', ( #17896 ), #16297, .T. ) ;
#7686 = CARTESIAN_POINT ( 'NONE',  ( -14.48388495494899963, 369.4323905683719431, 9.489475012073731008 ) ) ;
#7687 = DIRECTION ( 'NONE',  ( -1.000000000000000000, 0.000000000000000000, 0.000000000000000000 ) ) ;
#7688 = CARTESIAN_POINT ( 'NONE',  ( -10.20829729246300310, 496.3698905765655809, 7.653668647301790529 ) ) ;
#7689 = CARTESIAN_POINT ( 'NONE',  ( -25.35362745456398414, 386.6823905683720568, 16.75240474999998952 ) ) ;
#7690 = CARTESIAN_POINT ( 'NONE',  ( -44.16309181155855157, 235.9948905683720284, 6.410867750099241924 ) ) ;
#7691 = AXIS2_PLACEMENT_3D ( 'NONE', #17213, #18399, #10487 ) ;
#7692 = CARTESIAN_POINT ( 'NONE',  ( -35.09675569278795138, 411.9948905683720000, -15.47720386886985544 ) ) ;
#7693 = CARTESIAN_POINT ( 'NONE',  ( -45.64106924314017988, 322.9323905765655809, 11.32908994701042715 ) ) ;
#7694 = CARTESIAN_POINT ( 'NONE',  ( 8.938426032941704028E-16, 585.7448905601785327, 0.000000000000000000 ) ) ;
#7695 = CARTESIAN_POINT ( 'NONE',  ( -25.35362745456398414, 301.0573905683720568, -16.75240474999999307 ) ) ;
#7696 = CARTESIAN_POINT ( 'NONE',  ( -11.93348319268873148, 450.3698905683720000, -2.051577885510841163E-15 ) ) ;
#7697 = CARTESIAN_POINT ( 'NONE',  ( -11.73070664223725856, 461.3073905601784759, 11.32908994701042005 ) ) ;
#7698 = CARTESIAN_POINT ( 'NONE',  ( -11.73070664223724791, 371.3073905601784759, 11.32908994701042005 ) ) ;
#7699 = CARTESIAN_POINT ( 'NONE',  ( -28.68588794268874054, 573.2448905601785327, 0.000000000000000000 ) ) ;
#7700 = ADVANCED_FACE ( 'NONE', ( #19524 ), #13149, .F. ) ;
#7701 = AXIS2_PLACEMENT_3D ( 'NONE', #20118, #18058, #11680 ) ;
#7702 = CARTESIAN_POINT ( 'NONE',  ( -22.27502019258948707, 362.2448905683720000, -15.47720386886985544 ) ) ;
#7703 = CARTESIAN_POINT ( 'NONE',  ( -25.35362745456400901, 511.0573905683720568, -16.75240474999999307 ) ) ;
#7704 = AXIS2_PLACEMENT_3D ( 'NONE', #11854, #18551, #412 ) ;
#7705 = CARTESIAN_POINT ( 'NONE',  ( -45.64106924314020119, 516.3073905601784190, -11.32908994701042715 ) ) ;
#7706 = CARTESIAN_POINT ( 'NONE',  ( -28.68588794268871212, 331.3698905683720000, -16.75240474999999307 ) ) ;
#7707 = ORIENTED_EDGE ( 'NONE', *, *, #607, .F. ) ;
#7708 = CARTESIAN_POINT ( 'NONE',  ( 0.4037800551813705008, 4.058962678540093627, -5.969670414742685338 ) ) ;
#7709 = ORIENTED_EDGE ( 'NONE', *, *, #17690, .F. ) ;
#7710 = DIRECTION ( 'NONE',  ( -0.9997392892938121722, -0.02283316540262222971, 0.000000000000000000 ) ) ;
#7711 = ADVANCED_FACE ( 'NONE', ( #14464 ), #1470, .T. ) ;
#7712 = CARTESIAN_POINT ( 'NONE',  ( -40.53162694259544452, 414.1198905683720000, -11.84573899990672707 ) ) ;
#7713 = CARTESIAN_POINT ( 'NONE',  ( -38.17536295476246977, 452.3073905683720568, -14.20200298773971426 ) ) ;
#7714 = ORIENTED_EDGE ( 'NONE', *, *, #2479, .T. ) ;
#7715 = CARTESIAN_POINT ( 'NONE',  ( -32.01814843081345430, 461.6823905683720568, -16.75240474999999307 ) ) ;
#7716 = DIRECTION ( 'NONE',  ( 1.000000000000000000, 0.000000000000000000, 0.000000000000000000 ) ) ;
#7717 = DIRECTION ( 'NONE',  ( 1.000000000000000000, 0.000000000000000000, 0.000000000000000000 ) ) ;
#7718 = CARTESIAN_POINT ( 'NONE',  ( -42.82802356641966668, 410.7448905765656377, -14.14213562373094746 ) ) ;
#7719 = DIRECTION ( 'NONE',  ( 0.000000000000000000, 0.000000000000000000, 1.000000000000000000 ) ) ;
#7720 = DIRECTION ( 'NONE',  ( 0.000000000000000000, 1.000000000000000000, 0.000000000000000000 ) ) ;
#7721 = CYLINDRICAL_SURFACE ( 'NONE', #5638, 19.99999999999999645 ) ;
#7722 = LINE ( 'NONE', #17992, #10099 ) ;
#7723 = VECTOR ( 'NONE', #20420, 1000.000000000000000 ) ;
#7724 = DIRECTION ( 'NONE',  ( 0.000000000000000000, 0.000000000000000000, 1.000000000000000000 ) ) ;
#7725 = CARTESIAN_POINT ( 'NONE',  ( -8.685887942688710339, 256.9948905765655809, -2.449293598294705724E-15 ) ) ;
#7726 = CARTESIAN_POINT ( 'NONE',  ( 30.42502041961814996, 180.1716627696692967, -20.00000000000000355 ) ) ;
#7727 = CARTESIAN_POINT ( 'NONE',  ( -21.03221929538689849, 240.3698905601784759, 18.47759065022572500 ) ) ;
#7728 = DIRECTION ( 'NONE',  ( -0.6352526299242171604, 0.000000000000000000, -0.7723044064191046942 ) ) ;
#7729 = CARTESIAN_POINT ( 'NONE',  ( -11.93348319268872793, 420.3698905683720568, -2.051577885510841163E-15 ) ) ;
#7730 = CARTESIAN_POINT ( 'NONE',  ( -36.33955658999050797, 385.3698905601785327, -18.47759065022572855 ) ) ;
#7731 = CARTESIAN_POINT ( 'NONE',  ( -22.27502019258946220, 248.4948905683720284, 15.47720386886985189 ) ) ;
#7732 = ORIENTED_EDGE ( 'NONE', *, *, #19059, .T. ) ;
#7733 = EDGE_LOOP ( 'NONE', ( #17900, #17198, #20759, #7762 ) ) ;
#7734 = VERTEX_POINT ( 'NONE', #6214 ) ;
#7735 = CARTESIAN_POINT ( 'NONE',  ( -28.68588794268872277, 457.8698905683720000, 16.75240474999999307 ) ) ;
#7736 = CARTESIAN_POINT ( 'NONE',  ( -48.68588794268869435, 231.6823905765656377, -3.978247347593158345 ) ) ;
#7737 = AXIS2_PLACEMENT_3D ( 'NONE', #10286, #13878, #16906 ) ;
#7738 = EDGE_LOOP ( 'NONE', ( #2114, #184, #15688, #13403, #7940, #15079, #18691, #18537, #19710, #549, #12942, #20649 ) ) ;
#7739 = CARTESIAN_POINT ( 'NONE',  ( -24.70764059509556887, 524.8073905765658083, 19.99999999999998934 ) ) ;
#7740 = CARTESIAN_POINT ( 'NONE',  ( -25.35362745456397704, 231.0573905683720568, -16.75240474999999307 ) ) ;
#7741 = ORIENTED_EDGE ( 'NONE', *, *, #19490, .F. ) ;
#7742 = CARTESIAN_POINT ( 'NONE',  ( -28.68588794268873343, 526.3698905683720568, 16.75240474999999307 ) ) ;
#7743 = LINE ( 'NONE', #21374, #8656 ) ;
#7744 = CARTESIAN_POINT ( 'NONE',  ( -48.68588794268872277, 471.6823905765656377, -3.978247347593158345 ) ) ;
#7745 = CARTESIAN_POINT ( 'NONE',  ( 0.000000000000000000, 0.000000000000000000, 6.500000000000000000 ) ) ;
#7746 = SURFACE_STYLE_FILL_AREA ( #20853 ) ;
#7747 = CARTESIAN_POINT ( 'NONE',  ( -47.16347859291443001, 241.3698905765656093, -7.653668647301793193 ) ) ;
#7748 = CARTESIAN_POINT ( 'NONE',  ( -35.09675569278793716, 227.2448905683720568, 15.47720386886985366 ) ) ;
#7749 = DIRECTION ( 'NONE',  ( -1.000000000000000000, -0.000000000000000000, -0.000000000000000000 ) ) ;
#7750 = CARTESIAN_POINT ( 'NONE',  ( -11.93348319268870661, 228.5573905683720568, 3.332260488124728415 ) ) ;
#7751 = CARTESIAN_POINT ( 'NONE',  ( -16.84014894278198682, 321.6198905683720568, -11.84573899990672707 ) ) ;
#7752 = ADVANCED_FACE ( 'NONE', ( #4604 ), #21364, .T. ) ;
#7753 = CARTESIAN_POINT ( 'NONE',  ( -43.68588794268869435, 193.9102039777116602, 0.000000000000000000 ) ) ;
#7754 = CARTESIAN_POINT ( 'NONE',  ( -40.01497788969913216, 378.8073905601785327, 16.95518130045146776 ) ) ;
#7755 = EDGE_CURVE ( 'NONE', #13610, #12221, #7936, .T. ) ;
#7756 = CARTESIAN_POINT ( 'NONE',  ( -22.27502019258947996, 302.2448905683720000, -15.47720386886985544 ) ) ;
#7757 = ADVANCED_FACE ( 'NONE', ( #11518 ), #21152, .T. ) ;
#7758 = CARTESIAN_POINT ( 'NONE',  ( -11.93348319268872260, 378.8698905683720000, -2.051577885510841163E-15 ) ) ;
#7759 = CARTESIAN_POINT ( 'NONE',  ( -22.27502019258950483, 522.2448905683720568, -15.47720386886985544 ) ) ;
#7760 = CARTESIAN_POINT ( 'NONE',  ( -8.685887942688722774, 382.5573905601784759, -3.978247347593165895 ) ) ;
#7761 = CARTESIAN_POINT ( 'NONE',  ( -45.64106924314016567, 231.0573905765656093, -11.32908994701042538 ) ) ;
#7762 = ORIENTED_EDGE ( 'NONE', *, *, #662, .F. ) ;
#7763 = ORIENTED_EDGE ( 'NONE', *, *, #14612, .T. ) ;
#7764 = CARTESIAN_POINT ( 'NONE',  ( -32.01814843081346140, 493.1823905683721136, -16.75240474999999307 ) ) ;
#7765 = CARTESIAN_POINT ( 'NONE',  ( 6.416697501590670427, 217.7548513357008630, -45.00000000000000000 ) ) ;
#7766 = ORIENTED_EDGE ( 'NONE', *, *, #16765, .F. ) ;
#7767 = ADVANCED_FACE ( 'NONE', ( #9885 ), #5022, .T. ) ;
#7768 = CARTESIAN_POINT ( 'NONE',  ( -45.43829269268870519, 305.3698905683720568, 0.000000000000000000 ) ) ;
#7769 = CARTESIAN_POINT ( 'NONE',  ( -25.35362745456398770, 321.0573905683720568, -16.75240474999999307 ) ) ;
#7770 = CARTESIAN_POINT ( 'NONE',  ( -32.66413529028186247, 269.8073905765655809, -19.99999999999999289 ) ) ;
#7771 = CARTESIAN_POINT ( 'NONE',  ( -24.70764059509557242, 474.4323905601785327, -19.99999999999999289 ) ) ;
#7772 = DIRECTION ( 'NONE',  ( 0.000000000000000000, 1.000000000000000000, -0.000000000000000000 ) ) ;
#7773 = CARTESIAN_POINT ( 'NONE',  ( -25.35362745456398414, 388.1823905683720568, 16.75240474999998952 ) ) ;
#7774 = CARTESIAN_POINT ( 'NONE',  ( -41.83569717483972994, 326.0737056351150613, 24.99999999999998934 ) ) ;
#7775 = DIRECTION ( 'NONE',  ( 0.000000000000000000, -1.000000000000000000, 0.000000000000000000 ) ) ;
#7776 = CARTESIAN_POINT ( 'NONE',  ( -28.68588794268870146, 244.7448905601785043, -19.99999999999999289 ) ) ;
#7777 = CARTESIAN_POINT ( 'NONE',  ( -44.16309181155857289, 444.4948905683720568, 6.410867750099241924 ) ) ;
#7778 = DIRECTION ( 'NONE',  ( -0.000000000000000000, -0.000000000000000000, 1.000000000000000000 ) ) ;
#7779 = EDGE_LOOP ( 'NONE', ( #12548, #17248, #20353 ) ) ;
#7780 = CARTESIAN_POINT ( 'NONE',  ( -42.82802356641967378, 455.9948905601784759, -14.14213562373094746 ) ) ;
#7781 = ORIENTED_EDGE ( 'NONE', *, *, #7294, .F. ) ;
#7782 = ORIENTED_EDGE ( 'NONE', *, *, #16824, .T. ) ;
#7783 = EDGE_LOOP ( 'NONE', ( #4867, #14941, #21257, #569 ) ) ;
#7784 = DIRECTION ( 'NONE',  ( 0.000000000000000000, 0.000000000000000000, -1.000000000000000000 ) ) ;
#7785 = CARTESIAN_POINT ( 'NONE',  ( -45.64106924314017988, 326.3073905601785327, -11.32908994701042715 ) ) ;
#7786 = CARTESIAN_POINT ( 'NONE',  ( -39.89451704885674843, 223.9102039777116318, -12.46781227845250584 ) ) ;
#7787 = CARTESIAN_POINT ( 'NONE',  ( -14.48388495494899963, 361.3073905683720568, -9.489475012073734561 ) ) ;
#7788 = DIRECTION ( 'NONE',  ( -1.000000000000000000, -0.000000000000000000, -0.000000000000000000 ) ) ;
#7789 = CARTESIAN_POINT ( 'NONE',  ( -14.54375231895778420, 495.7448905765656377, 14.14213562373094568 ) ) ;
#7790 = CARTESIAN_POINT ( 'NONE',  ( -14.48388495494900496, 389.8073905683721136, -9.489475012073736337 ) ) ;
#7791 = CARTESIAN_POINT ( 'NONE',  ( -25.35362745456397349, 222.5573905683720568, -16.75240474999999307 ) ) ;
#7792 = CARTESIAN_POINT ( 'NONE',  ( -16.84014894278199748, 410.1198905683720000, -11.84573899990672707 ) ) ;
#7793 = SHAPE_REPRESENTATION ( 'Reciprocating Press Ram Head', ( #12794 ), #14195 ) ;
#7794 = CARTESIAN_POINT ( 'NONE',  ( -32.66413529028187668, 329.8073905765655809, -19.99999999999999289 ) ) ;
#7795 = LINE ( 'NONE', #20478, #18265 ) ;
#7796 = CARTESIAN_POINT ( 'NONE',  ( -11.93348319268871371, 299.1823905683720000, -3.332260488124732856 ) ) ;
#7797 = CARTESIAN_POINT ( 'NONE',  ( -35.09675569278795848, 463.4948905683720000, -15.47720386886985544 ) ) ;
#7798 = CARTESIAN_POINT ( 'NONE',  ( -47.16347859291445843, 457.8698905601785327, 7.653668647301805628 ) ) ;
#7799 = CARTESIAN_POINT ( 'NONE',  ( -32.66413529028186957, 369.4323905601784190, 19.99999999999999289 ) ) ;
#7800 = CARTESIAN_POINT ( 'NONE',  ( 0.000000000000000000, 0.000000000000000000, 0.000000000000000000 ) ) ;
#7801 = ADVANCED_FACE ( 'NONE', ( #14424 ), #13217, .T. ) ;
#7802 = CARTESIAN_POINT ( 'NONE',  ( -28.68588794268871212, 367.8698905683720000, 16.75240474999999307 ) ) ;
#7803 = CARTESIAN_POINT ( 'NONE',  ( -11.93348319268873858, 498.5573905683720568, 3.332260488124728415 ) ) ;
#7804 = CARTESIAN_POINT ( 'NONE',  ( -8.685887942688740537, 511.9323905601785327, 3.978247347593161010 ) ) ;
#7805 = CARTESIAN_POINT ( 'NONE',  ( -44.16309181155855867, 314.4948905683720000, 6.410867750099241924 ) ) ;
#7806 = AXIS2_PLACEMENT_3D ( 'NONE', #14109, #14217, #20804 ) ;
#7807 = VERTEX_POINT ( 'NONE', #19584 ) ;
#7808 = CARTESIAN_POINT ( 'NONE',  ( -24.70764059509557953, 524.4323905601783053, -19.99999999999999289 ) ) ;
#7809 = ORIENTED_EDGE ( 'NONE', *, *, #17226, .T. ) ;
#7810 = EDGE_CURVE ( 'NONE', #6752, #18462, #6855, .T. ) ;
#7811 = DIRECTION ( 'NONE',  ( -0.000000000000000000, -1.000000000000000000, -0.000000000000000000 ) ) ;
#7812 = CIRCLE ( 'NONE', #3670, 53.46661168214943416 ) ;
#7813 = CARTESIAN_POINT ( 'NONE',  ( -19.19641293061498999, 431.9323905683719431, -14.20200298773971603 ) ) ;
#7814 = CARTESIAN_POINT ( 'NONE',  ( -24.70764059509555111, 394.8073905765655809, 19.99999999999998934 ) ) ;
#7815 = CARTESIAN_POINT ( 'NONE',  ( -28.68588794268872277, 436.3698905683720000, 16.75240474999999307 ) ) ;
#7816 = EDGE_LOOP ( 'NONE', ( #7444, #9473, #10207, #9619 ) ) ;
#7817 = CARTESIAN_POINT ( 'NONE',  ( -40.53162694259545162, 462.6198905683720000, -11.84573899990672707 ) ) ;
#7818 = DIRECTION ( 'NONE',  ( 0.000000000000000000, 0.000000000000000000, 1.000000000000000000 ) ) ;
#7819 = DIRECTION ( 'NONE',  ( 1.000000000000000000, 0.000000000000000000, 0.000000000000000000 ) ) ;
#7820 = CARTESIAN_POINT ( 'NONE',  ( -24.70764059509556532, 389.1823905765656377, -19.99999999999999289 ) ) ;
#7821 = CARTESIAN_POINT ( 'NONE',  ( 81.24038404635965094, 30.52886280891152282, 131.1729372809869005 ) ) ;
#7822 = DIRECTION ( 'NONE',  ( -1.000000000000000000, 0.000000000000000000, 0.000000000000000000 ) ) ;
#7823 = CARTESIAN_POINT ( 'NONE',  ( 0.01372220897661586593, 5.309964801958114045, -3.802871176606130277 ) ) ;
#7824 = CARTESIAN_POINT ( 'NONE',  ( -24.70764059509553334, 254.8073905765656093, 19.99999999999998934 ) ) ;
#7825 = AXIS2_PLACEMENT_3D ( 'NONE', #11296, #9464, #16076 ) ;
#7826 = CARTESIAN_POINT ( 'NONE',  ( 2.416697501590669095, 217.7548513357008630, -60.00000000000000000 ) ) ;
#7827 = CARTESIAN_POINT ( 'NONE',  ( -32.66413529028185536, 255.0573905601785043, -19.99999999999999289 ) ) ;
#7828 = CARTESIAN_POINT ( 'NONE',  ( -36.33955658999050797, 345.3698905601784759, -18.47759065022572855 ) ) ;
#7829 = ADVANCED_FACE ( 'NONE', ( #12893 ), #11254, .T. ) ;
#7830 = VECTOR ( 'NONE', #20482, 1000.000000000000114 ) ;
#7831 = CARTESIAN_POINT ( 'NONE',  ( -40.53162694259544452, 426.6198905683720000, 11.84573899990672885 ) ) ;
#7832 = CARTESIAN_POINT ( 'NONE',  ( -8.685887942688887975, 266.6823905765656377, 3.978247347593586447 ) ) ;
#7833 = CARTESIAN_POINT ( 'NONE',  ( -22.27502019258947286, 242.2448905683720000, -15.47720386886985544 ) ) ;
#7834 = ORIENTED_EDGE ( 'NONE', *, *, #20524, .F. ) ;
#7835 = ORIENTED_EDGE ( 'NONE', *, *, #3737, .T. ) ;
#7836 = DIRECTION ( 'NONE',  ( 0.000000000000000000, 1.000000000000000000, 0.000000000000000000 ) ) ;
#7837 = ORIENTED_EDGE ( 'NONE', *, *, #19528, .F. ) ;
#7838 = CARTESIAN_POINT ( 'NONE',  ( -25.35362745456399480, 468.1823905683720568, 16.75240474999998952 ) ) ;
#7839 = CARTESIAN_POINT ( 'NONE',  ( -28.68588794268869790, 234.4948905765656377, 19.99999999999999289 ) ) ;
#7840 = ORIENTED_EDGE ( 'NONE', *, *, #4197, .T. ) ;
#7841 = DIRECTION ( 'NONE',  ( 0.000000000000000000, -1.000000000000000000, 0.000000000000000000 ) ) ;
#7842 = CARTESIAN_POINT ( 'NONE',  ( -40.53162694259545873, 534.1198905683720568, -11.84573899990672707 ) ) ;
#7843 = ORIENTED_EDGE ( 'NONE', *, *, #7810, .F. ) ;
#7844 = CARTESIAN_POINT ( 'NONE',  ( -25.35362745456400191, 526.6823905683720568, 16.75240474999998952 ) ) ;
#7845 = FACE_OUTER_BOUND ( 'NONE', #9778, .T. ) ;
#7846 = ADVANCED_FACE ( 'NONE', ( #4452, #16461 ), #19689, .F. ) ;
#7847 = AXIS2_PLACEMENT_3D ( 'NONE', #17108, #8867, #15067 ) ;
#7848 = CARTESIAN_POINT ( 'NONE',  ( -14.54375231895778064, 448.2448905765656377, -14.14213562373094746 ) ) ;
#7849 = CARTESIAN_POINT ( 'NONE',  ( -8.685887942688720997, 352.2448905601784759, -2.449293598294705724E-15 ) ) ;
#7850 = CARTESIAN_POINT ( 'NONE',  ( -48.68588794268870146, 281.9948905765656377, 0.000000000000000000 ) ) ;
#7851 = CARTESIAN_POINT ( 'NONE',  ( -8.685887942688708563, 236.9948905765656377, -2.449293598294705724E-15 ) ) ;
#7852 = FACE_OUTER_BOUND ( 'NONE', #18272, .T. ) ;
#7853 = CARTESIAN_POINT ( 'NONE',  ( -12.66381623556490332, 223.9102039777117454, 12.07890426730769029 ) ) ;
#7854 = CARTESIAN_POINT ( 'NONE',  ( -22.27502019258945865, 226.9948905683720284, 15.47720386886985189 ) ) ;
#7855 = CARTESIAN_POINT ( 'NONE',  ( -16.84014894278197971, 309.1198905683720000, 11.84573899990672530 ) ) ;
#7856 = EDGE_CURVE ( 'NONE', #11704, #18039, #8000, .T. ) ;
#7857 = CARTESIAN_POINT ( 'NONE',  ( -8.685887942688729879, 442.2448905601785327, -2.449293598294705724E-15 ) ) ;
#7858 = DIRECTION ( 'NONE',  ( 1.000000000000000000, 0.000000000000000000, 0.000000000000000000 ) ) ;
#7859 = CARTESIAN_POINT ( 'NONE',  ( -45.43829269268870519, 305.3698905683720568, 0.000000000000000000 ) ) ;
#7860 = CARTESIAN_POINT ( 'NONE',  ( -45.43829269268870519, 374.1823905683720568, 3.332260488124734632 ) ) ;
#7861 = CARTESIAN_POINT ( 'NONE',  ( -14.48388495494901562, 519.4323905683719431, 9.489475012073731008 ) ) ;
#7862 = CARTESIAN_POINT ( 'NONE',  ( -24.70764059509556176, 374.4323905601784759, -19.99999999999999289 ) ) ;
#7863 = CARTESIAN_POINT ( 'NONE',  ( -10.20829729246299067, 402.8698905601784759, -7.653668647301794969 ) ) ;
#7864 = VERTEX_POINT ( 'NONE', #9423 ) ;
#7865 = CARTESIAN_POINT ( 'NONE',  ( -32.01814843081346140, 487.5573905683720568, 16.75240474999999307 ) ) ;
#7866 = PLANE ( 'NONE',  #14929 ) ;
#7867 = CARTESIAN_POINT ( 'NONE',  ( -16.84014894278197616, 277.6198905683720568, 11.84573899990672530 ) ) ;
#7868 = EDGE_LOOP ( 'NONE', ( #17975, #13322, #20241, #1477 ) ) ;
#7869 = CARTESIAN_POINT ( 'NONE',  ( -22.27502019258947641, 282.2448905683720568, -15.47720386886985544 ) ) ;
#7870 = CARTESIAN_POINT ( 'NONE',  ( -14.48388495494899253, 317.9323905683720000, 9.489475012073732785 ) ) ;
#7871 = CARTESIAN_POINT ( 'NONE',  ( -14.54375231895775933, 268.2448905765656377, -14.14213562373094746 ) ) ;
#7872 = CARTESIAN_POINT ( 'NONE',  ( -21.03221929538693757, 474.1198905601784759, -18.47759065022572855 ) ) ;
#7873 = CARTESIAN_POINT ( 'NONE',  ( -35.09675569278793006, 231.9948905683720284, -15.47720386886985544 ) ) ;
#7874 = CARTESIAN_POINT ( 'NONE',  ( -42.88789093042843348, 376.3073905683720000, 9.489475012073736337 ) ) ;
#7875 = CARTESIAN_POINT ( 'NONE',  ( -42.87299489053027912, 204.0036020648173292, 4.871053504435129078 ) ) ;
#7876 = CARTESIAN_POINT ( 'NONE',  ( 5.299999999999999822, -7.505553499465150047, 0.000000000000000000 ) ) ;
#7877 = EDGE_CURVE ( 'NONE', #10847, #1235, #13886, .T. ) ;
#7878 = DIRECTION ( 'NONE',  ( 0.000000000000000000, 0.000000000000000000, 1.000000000000000000 ) ) ;
#7879 = AXIS2_PLACEMENT_3D ( 'NONE', #6532, #9570, #16509 ) ;
#7880 = ADVANCED_FACE ( 'NONE', ( #15244 ), #8835, .F. ) ;
#7881 = CARTESIAN_POINT ( 'NONE',  ( -13.20868407381886733, 438.2448905683720000, 6.410867750099229490 ) ) ;
#7882 = CARTESIAN_POINT ( 'NONE',  ( 6.416697501590670427, 217.7548513357008630, 45.00000000000000000 ) ) ;
#7883 = ORIENTED_EDGE ( 'NONE', *, *, #10215, .T. ) ;
#7884 = CARTESIAN_POINT ( 'NONE',  ( -42.82802356641966668, 435.9948905601784759, -14.14213562373094746 ) ) ;
#7885 = ORIENTED_EDGE ( 'NONE', *, *, #20200, .T. ) ;
#7886 = ORIENTED_EDGE ( 'NONE', *, *, #7005, .F. ) ;
#7887 = ORIENTED_EDGE ( 'NONE', *, *, #13857, .T. ) ;
#7888 = CARTESIAN_POINT ( 'NONE',  ( -42.82802356641964536, 205.1437886375728965, -5.000000000000001776 ) ) ;
#7889 = CARTESIAN_POINT ( 'NONE',  ( -21.03221929538691981, 324.1198905601784759, -18.47759065022572855 ) ) ;
#7890 = LINE ( 'NONE', #20279, #13820 ) ;
#7891 = CARTESIAN_POINT ( 'NONE',  ( -22.27502019258947641, 348.4948905683720000, 15.47720386886985189 ) ) ;
#7892 = CARTESIAN_POINT ( 'NONE',  ( -42.82802356641967378, 500.7448905765656946, -14.14213562373094746 ) ) ;
#7893 = CARTESIAN_POINT ( 'NONE',  ( -40.53162694259544452, 392.6198905683720568, -11.84573899990672707 ) ) ;
#7894 = DIRECTION ( 'NONE',  ( 0.000000000000000000, -1.000000000000000000, 0.000000000000000000 ) ) ;
#7895 = CARTESIAN_POINT ( 'NONE',  ( -13.20868407381886200, 379.4948905683720000, -6.410867750099233042 ) ) ;
#7896 = AXIS2_PLACEMENT_3D ( 'NONE', #6518, #17784, #3075 ) ;
#7897 = CARTESIAN_POINT ( 'NONE',  ( -24.70764059509555821, 329.1823905765656377, -19.99999999999999289 ) ) ;
#7898 = CARTESIAN_POINT ( 'NONE',  ( -35.09675569278793716, 281.9948905683720000, -15.47720386886985544 ) ) ;
#7899 = ADVANCED_BREP_SHAPE_REPRESENTATION ( '', ( #12161, #12794 ), #14195 ) ;
#7900 = CARTESIAN_POINT ( 'NONE',  ( -45.43829269268871229, 435.6823905683720568, 3.332260488124734632 ) ) ;
#7901 = CARTESIAN_POINT ( 'NONE',  ( -28.68588794268872633, 250.8848358243226357, 0.000000000000000000 ) ) ;
#7902 = CARTESIAN_POINT ( 'NONE',  ( -47.16347859291444422, 367.8698905601784759, 7.653668647301805628 ) ) ;
#7903 = AXIS2_PLACEMENT_3D ( 'NONE', #6225, #12840, #19535 ) ;
#7904 = FACE_OUTER_BOUND ( 'NONE', #19346, .T. ) ;
#7905 = CARTESIAN_POINT ( 'NONE',  ( -19.19641293061498288, 341.9323905683720568, -14.20200298773971603 ) ) ;
#7906 = CARTESIAN_POINT ( 'NONE',  ( -28.68588794268873343, 511.3698905683720000, -16.75240474999999307 ) ) ;
#7907 = CARTESIAN_POINT ( 'NONE',  ( -42.82802356641968089, 508.4948905601784759, 14.14213562373094923 ) ) ;
#7908 = CARTESIAN_POINT ( 'NONE',  ( -19.19641293061497933, 327.3073905683720568, 14.20200298773971426 ) ) ;
#7909 = ORIENTED_EDGE ( 'NONE', *, *, #12457, .T. ) ;
#7910 = CARTESIAN_POINT ( 'NONE',  ( -32.66413529028189089, 525.0573905601785327, -19.99999999999999289 ) ) ;
#7911 = ORIENTED_EDGE ( 'NONE', *, *, #5141, .T. ) ;
#7912 = DIRECTION ( 'NONE',  ( 0.000000000000000000, -1.000000000000000000, 0.000000000000000000 ) ) ;
#7913 =( BOUNDED_CURVE ( )  B_SPLINE_CURVE ( 2, ( #4334, #9189, #10915, #20781, #999, #17318, #7676, #4110, #7776, #5947, #15815, #20666, #19158, #9409, #7564, #16025, #20885 ),
 .UNSPECIFIED., .F., .T. ) 
 B_SPLINE_CURVE_WITH_KNOTS ( ( 3, 2, 2, 2, 2, 2, 2, 2, 3 ),
 ( 0.9062500000000001110, 0.9082031250000001110, 0.9101562500000001110, 0.9121093750000001110, 0.9140625000000001110, 0.9160156250000001110, 0.9179687500000001110, 0.9199218750000001110, 0.9218750000000001110 ),
 .UNSPECIFIED. ) 
 CURVE ( )  GEOMETRIC_REPRESENTATION_ITEM ( )  RATIONAL_B_SPLINE_CURVE ( ( 0.9999999999999988898, 0.9807852804032315408, 1.000000000000000000, 0.9807852804032304306, 1.000000000000000000, 0.9807852804032304306, 1.000000000000000000, 0.9807852804032304306, 1.000000000000000000, 0.9807852804032304306, 1.000000000000000000, 0.9807852804032304306, 1.000000000000000000, 0.9807852804032304306, 1.000000000000000000, 0.9807852804032293204, 1.000000000000001110 ) ) 
 REPRESENTATION_ITEM ( '' )  );
#7914 = CARTESIAN_POINT ( 'NONE',  ( -25.35362745456399836, 422.5573905683721136, -16.75240474999999307 ) ) ;
#7915 = FACE_OUTER_BOUND ( 'NONE', #6864, .T. ) ;
#7916 = LINE ( 'NONE', #3069, #15233 ) ;
#7917 = CARTESIAN_POINT ( 'NONE',  ( -16.84014894278200103, 450.1198905683720568, -11.84573899990672707 ) ) ;
#7918 = EDGE_LOOP ( 'NONE', ( #4612, #11403, #3595, #18505 ) ) ;
#7919 = CARTESIAN_POINT ( 'NONE',  ( -25.35362745456400191, 451.0573905683719431, -16.75240474999999307 ) ) ;
#7920 = CARTESIAN_POINT ( 'NONE',  ( 60.03793209889851568, 36.20386280891151642, 131.1729372809869005 ) ) ;
#7921 = DIRECTION ( 'NONE',  ( -0.000000000000000000, -0.000000000000000000, -1.000000000000000000 ) ) ;
#7922 = CARTESIAN_POINT ( 'NONE',  ( -32.66413529028187668, 379.8073905765656377, -19.99999999999999289 ) ) ;
#7923 = DIRECTION ( 'NONE',  ( 0.000000000000000000, 0.000000000000000000, 1.000000000000000000 ) ) ;
#7924 = CARTESIAN_POINT ( 'NONE',  ( 4.700000000000000178, 7.505553499465139389, 0.000000000000000000 ) ) ;
#7925 = CARTESIAN_POINT ( 'NONE',  ( -49.57497958038184294, -6.743947802724785386E-15, 0.000000000000000000 ) ) ;
#7926 = CARTESIAN_POINT ( 'NONE',  ( -40.01497788969911795, 253.5573905765656093, 16.95518130045146776 ) ) ;
#7927 = CARTESIAN_POINT ( 'NONE',  ( -40.53162694259545873, 516.6198905683720568, 11.84573899990672885 ) ) ;
#7928 = DIRECTION ( 'NONE',  ( 0.000000000000000000, 0.000000000000000000, 1.000000000000000000 ) ) ;
#7929 = CARTESIAN_POINT ( 'NONE',  ( -8.685887942688530927, 252.5573905601784475, -3.978247347592740013 ) ) ;
#7930 = CARTESIAN_POINT ( 'NONE',  ( -8.685887942688728103, 422.2448905601784759, -2.449293598294705724E-15 ) ) ;
#7931 = CARTESIAN_POINT ( 'NONE',  ( -11.93348319268872970, 430.0573905683721136, 3.332260488124728415 ) ) ;
#7932 = CARTESIAN_POINT ( 'NONE',  ( -17.35679799567827786, 265.4323905765656377, 16.95518130045146421 ) ) ;
#7933 = AXIS2_PLACEMENT_3D ( 'NONE', #4150, #13689, #2328 ) ;
#7934 = CARTESIAN_POINT ( 'NONE',  ( -11.93348319268870661, 240.3698905683720568, -2.051577885510841163E-15 ) ) ;
#7935 = ORIENTED_EDGE ( 'NONE', *, *, #10844, .T. ) ;
#7936 = LINE ( 'NONE', #4921, #15848 ) ;
#7937 = EDGE_LOOP ( 'NONE', ( #13340, #16672, #10855, #14834 ) ) ;
#7938 = CARTESIAN_POINT ( 'NONE',  ( -38.17536295476246266, 466.9323905683721136, 14.20200298773971781 ) ) ;
#7939 = CARTESIAN_POINT ( 'NONE',  ( -45.43829269268873361, 533.8698905683720568, 0.000000000000000000 ) ) ;
#7940 = ORIENTED_EDGE ( 'NONE', *, *, #16463, .T. ) ;
#7941 = CARTESIAN_POINT ( 'NONE',  ( -8.685887942688742314, 573.2448905601785327, 2.449293598294706119E-15 ) ) ;
#7942 = CARTESIAN_POINT ( 'NONE',  ( -11.93348319268874214, 530.0573905683720568, 3.332260488124728415 ) ) ;
#7943 = ORIENTED_EDGE ( 'NONE', *, *, #5318, .T. ) ;
#7944 = CARTESIAN_POINT ( 'NONE',  ( -35.09675569278797269, 525.7448905683720568, 15.47720386886985366 ) ) ;
#7945 = CARTESIAN_POINT ( 'NONE',  ( 154.7587007620219026, 610.7448905601785327, 10.81142786866622885 ) ) ;
#7946 = EDGE_CURVE ( 'NONE', #13150, #11401, #18583, .T. ) ;
#7947 = MECHANICAL_DESIGN_GEOMETRIC_PRESENTATION_REPRESENTATION (  '', ( #12459 ), #390 ) ;
#7948 = CARTESIAN_POINT ( 'NONE',  ( -42.82802356641966668, 440.7448905765656377, -14.14213562373094746 ) ) ;
#7949 = DIRECTION ( 'NONE',  ( 0.000000000000000000, -1.000000000000000000, 0.000000000000000000 ) ) ;
#7950 = CARTESIAN_POINT ( 'NONE',  ( -13.20868407381885845, 339.4948905683720568, -6.410867750099233042 ) ) ;
#7951 = CARTESIAN_POINT ( 'NONE',  ( -8.685887942688733432, 456.9948905765656377, -2.449293598294705724E-15 ) ) ;
#7952 = AXIS2_PLACEMENT_3D ( 'NONE', #5005, #20041, #8127 ) ;
#7953 = DIRECTION ( 'NONE',  ( 0.000000000000000000, 0.000000000000000000, 1.000000000000000000 ) ) ;
#7954 = LINE ( 'NONE', #4720, #15008 ) ;
#7955 = LINE ( 'NONE', #21170, #17343 ) ;
#7956 = CARTESIAN_POINT ( 'NONE',  ( -25.35362745456396638, 236.6823905683720284, 16.75240474999998952 ) ) ;
#7957 = AXIS2_PLACEMENT_3D ( 'NONE', #19429, #11411, #6123 ) ;
#7958 = CARTESIAN_POINT ( 'NONE',  ( -14.48388495494899253, 319.4323905683720568, 9.489475012073732785 ) ) ;
#7959 = CARTESIAN_POINT ( 'NONE',  ( -45.64106924314018698, 446.3073905601784190, -11.32908994701042538 ) ) ;
#7960 = CARTESIAN_POINT ( 'NONE',  ( -8.685887942688728103, 416.9948905765656377, -2.449293598294705724E-15 ) ) ;
#7961 = CARTESIAN_POINT ( 'NONE',  ( -16.84014894278197971, 299.1198905683720000, 11.84573899990672530 ) ) ;
#7962 = EDGE_CURVE ( 'NONE', #14472, #16345, #8171, .T. ) ;
#7963 = AXIS2_PLACEMENT_3D ( 'NONE', #6661, #8169, #8278 ) ;
#7964 = CARTESIAN_POINT ( 'NONE',  ( -45.43829269268870519, 364.1823905683720568, 3.332260488124734632 ) ) ;
#7965 = VECTOR ( 'NONE', #12584, 1000.000000000000114 ) ;
#7966 = CARTESIAN_POINT ( 'NONE',  ( -11.93348319268874214, 530.3698905683720568, -2.051577885510841163E-15 ) ) ;
#7967 = CARTESIAN_POINT ( 'NONE',  ( -10.20829729246298712, 372.8698905601784759, -7.653668647301794969 ) ) ;
#7968 = FACE_OUTER_BOUND ( 'NONE', #10899, .T. ) ;
#7969 = ORIENTED_EDGE ( 'NONE', *, *, #17936, .T. ) ;
#7970 = CARTESIAN_POINT ( 'NONE',  ( -35.09675569278795848, 493.4948905683720568, -15.47720386886985544 ) ) ;
#7971 = DIRECTION ( 'NONE',  ( 0.000000000000000000, -0.000000000000000000, -1.000000000000000000 ) ) ;
#7972 = CARTESIAN_POINT ( 'NONE',  ( -14.48388495494898898, 287.9323905683720000, 9.489475012073732785 ) ) ;
#7973 = AXIS2_PLACEMENT_3D ( 'NONE', #20312, #17073, #18468 ) ;
#7974 = ORIENTED_EDGE ( 'NONE', *, *, #21080, .T. ) ;
#7975 = ADVANCED_FACE ( 'NONE', ( #5486 ), #16970, .T. ) ;
#7976 = CARTESIAN_POINT ( 'NONE',  ( -28.68588794268870856, 292.8698905683720568, -16.75240474999999307 ) ) ;
#7977 = CARTESIAN_POINT ( 'NONE',  ( -44.16309181155857289, 333.2448905683720568, -6.410867750099231266 ) ) ;
#7978 = CARTESIAN_POINT ( 'NONE',  ( -47.16347859291443001, 262.6198905765655809, 7.653668647301805628 ) ) ;
#7979 = CARTESIAN_POINT ( 'NONE',  ( -32.66413529028188378, 475.0573905601785327, -19.99999999999999289 ) ) ;
#7980 = AXIS2_PLACEMENT_3D ( 'NONE', #19345, #17302, #768 ) ;
#7981 = LINE ( 'NONE', #14609, #20639 ) ;
#7982 = CARTESIAN_POINT ( 'NONE',  ( -18.66797547166049753, 223.9102039777116602, -17.31025331282116397 ) ) ;
#7983 = CARTESIAN_POINT ( 'NONE',  ( -28.68588794268871567, 377.8698905683720000, 16.75240474999999307 ) ) ;
#7984 = CARTESIAN_POINT ( 'NONE',  ( 0.000000000000000000, 610.7448905601785327, 0.000000000000000000 ) ) ;
#7985 = CARTESIAN_POINT ( 'NONE',  ( -48.68588794268857356, 461.6823905765656377, -3.978247347593530936 ) ) ;
#7986 = CARTESIAN_POINT ( 'NONE',  ( 0.000000000000000000, 0.000000000000000000, 0.000000000000000000 ) ) ;
#7987 = CARTESIAN_POINT ( 'NONE',  ( -45.43829269268871940, 413.8698905683720568, 0.000000000000000000 ) ) ;
#7988 = CYLINDRICAL_SURFACE ( 'NONE', #10657, 18.29169339157296648 ) ;
#7989 = VERTEX_POINT ( 'NONE', #2150 ) ;
#7990 = CARTESIAN_POINT ( 'NONE',  ( -48.68588794268871567, 417.2448905601784759, 0.000000000000000000 ) ) ;
#7991 = ORIENTED_EDGE ( 'NONE', *, *, #1303, .F. ) ;
#7992 = VERTEX_POINT ( 'NONE', #749 ) ;
#7993 = DIRECTION ( 'NONE',  ( 1.000000000000000000, 0.000000000000000000, 0.000000000000000000 ) ) ;
#7994 = CARTESIAN_POINT ( 'NONE',  ( -24.70764059509555466, 314.4323905601784190, -19.99999999999999289 ) ) ;
#7995 = CYLINDRICAL_SURFACE ( 'NONE', #20096, 19.99999999999999645 ) ;
#7996 = COLOUR_RGB ( '',0.7921568627450980005, 0.8196078431372548767, 0.9333333333333333481 ) ;
#7997 = CARTESIAN_POINT ( 'NONE',  ( -45.43829269268871229, 345.0573905683720568, -3.332260488124726638 ) ) ;
#7998 = CARTESIAN_POINT ( 'NONE',  ( -47.16347859291445843, 501.3698905765655809, -7.653668647301793193 ) ) ;
#7999 = CARTESIAN_POINT ( 'NONE',  ( -40.53162694259543741, 382.6198905683720568, -11.84573899990672707 ) ) ;
#8000 = LINE ( 'NONE', #17956, #20325 ) ;
#8001 = CARTESIAN_POINT ( 'NONE',  ( -25.35362745456399480, 381.0573905683719431, -16.75240474999999307 ) ) ;
#8002 = CARTESIAN_POINT ( 'NONE',  ( -47.16347859291444422, 331.3698905765656377, -7.653668647301793193 ) ) ;
#8003 = CARTESIAN_POINT ( 'NONE',  ( -47.16347859291445133, 426.6198905601785327, -7.653668647301793193 ) ) ;
#8004 = CARTESIAN_POINT ( 'NONE',  ( -45.43829269268870519, 283.5573905683721136, -3.332260488124726638 ) ) ;
#8005 = CARTESIAN_POINT ( 'NONE',  ( -45.43829269268871229, 435.0573905683720568, -3.332260488124726194 ) ) ;
#8006 = CARTESIAN_POINT ( 'NONE',  ( 3.458603197740078627, 135.1716627696692683, 33.59072564020503648 ) ) ;
#8007 = CARTESIAN_POINT ( 'NONE',  ( 0.2578475836320706649, 6.890627091270370208, 1.065083781909172966 ) ) ;
#8008 = CARTESIAN_POINT ( 'NONE',  ( 0.000000000000000000, 7.511572993685794170E-16, -6.499999999999999112 ) ) ;
#8009 = VECTOR ( 'NONE', #13211, 1000.000000000000000 ) ;
#8010 = EDGE_CURVE ( 'NONE', #20333, #2560, #20531, .T. ) ;
#8011 = CARTESIAN_POINT ( 'NONE',  ( -32.01814843081344719, 353.1823905683720568, -16.75240474999999307 ) ) ;
#8012 = CARTESIAN_POINT ( 'NONE',  ( -28.68588794268872633, 486.3698905683720568, 16.75240474999999307 ) ) ;
#8013 = EDGE_CURVE ( 'NONE', #13314, #14150, #16606, .T. ) ;
#8014 = CARTESIAN_POINT ( 'NONE',  ( -47.16347859291445843, 477.8698905601784759, 7.653668647301805628 ) ) ;
#8015 = CARTESIAN_POINT ( 'NONE',  ( -28.68588794268870856, 316.3698905683720568, 16.75240474999999307 ) ) ;
#8016 = ADVANCED_FACE ( 'NONE', ( #857 ), #10240, .T. ) ;
#8017 = ORIENTED_EDGE ( 'NONE', *, *, #774, .F. ) ;
#8018 = CARTESIAN_POINT ( 'NONE',  ( 72.94945500224395118, 285.0140030772282103, 20.00000000000000355 ) ) ;
#8019 = PRODUCT ( 'hex bolt gradec_iso_ISO 4016 - M8 x 40 x 22-WN', 'hex bolt gradec_iso_ISO 4016 - M8 x 40 x 22-WN', '', ( #14978 ) ) ;
#8020 = ORIENTED_EDGE ( 'NONE', *, *, #10448, .F. ) ;
#8021 = DIRECTION ( 'NONE',  ( -0.000000000000000000, -0.000000000000000000, -1.000000000000000000 ) ) ;
#8022 = VECTOR ( 'NONE', #8165, 1000.000000000000000 ) ;
#8023 = CARTESIAN_POINT ( 'NONE',  ( -22.27502019258949417, 412.2448905683720568, -15.47720386886985544 ) ) ;
#8024 = CARTESIAN_POINT ( 'NONE',  ( -8.685887942688726326, 396.9948905765656377, -2.449293598294705724E-15 ) ) ;
#8025 = CARTESIAN_POINT ( 'NONE',  ( -25.35362745456399125, 446.6823905683720568, 16.75240474999998952 ) ) ;
#8026 = CARTESIAN_POINT ( 'NONE',  ( -32.01814843081344719, 446.0573905683720000, 16.75240474999999307 ) ) ;
#8027 = CARTESIAN_POINT ( 'NONE',  ( 6.416697501590664210, 172.9933428177121186, -72.61850154709787830 ) ) ;
#8028 = DIRECTION ( 'NONE',  ( -0.1639927121256943288, 0.000000000000000000, -0.9864615503757149240 ) ) ;
#8029 = B_SPLINE_CURVE_WITH_KNOTS ( 'NONE', 1,
 ( #10172, #8551 ),
 .UNSPECIFIED., .F., .F.,
 ( 2, 2 ),
 ( 0.000000000000000000, 1.000000000000000000 ),
 .UNSPECIFIED. ) ;
#8030 = EDGE_CURVE ( 'NONE', #7734, #8775, #15564, .T. ) ;
#8031 = CARTESIAN_POINT ( 'NONE',  ( -47.16347859291444422, 381.3698905765656377, -7.653668647301793193 ) ) ;
#8032 = CARTESIAN_POINT ( 'NONE',  ( 115.7989814974898195, 160.1716627696691830, -20.00000000000000355 ) ) ;
#8033 = CARTESIAN_POINT ( 'NONE',  ( -40.01497788969914637, 390.4323905765656377, -16.95518130045146421 ) ) ;
#8034 = FACE_OUTER_BOUND ( 'NONE', #4707, .T. ) ;
#8035 = VECTOR ( 'NONE', #8463, 1000.000000000000000 ) ;
#8036 = CARTESIAN_POINT ( 'NONE',  ( 65.85920792673738333, 160.1716627696692683, 20.00000000000000355 ) ) ;
#8037 = CARTESIAN_POINT ( 'NONE',  ( -28.68588794268872988, 497.8698905683720568, 16.75240474999999307 ) ) ;
#8038 = FACE_OUTER_BOUND ( 'NONE', #16777, .T. ) ;
#8039 = LINE ( 'NONE', #19517, #13895 ) ;
#8040 = CARTESIAN_POINT ( 'NONE',  ( -8.685887942689062058, 521.9323905601784190, 3.978247347593932837 ) ) ;
#8041 = CARTESIAN_POINT ( 'NONE',  ( -40.53162694259544452, 414.1198905683720000, -11.84573899990672707 ) ) ;
#8042 = CYLINDRICAL_SURFACE ( 'NONE', #13009, 19.99999999999999645 ) ;
#8043 =( BOUNDED_CURVE ( )  B_SPLINE_CURVE ( 2, ( #14854, #20028, #18182, #11699, #6604, #18291, #3478, #8444, #11479, #253, #5204, #18077, #19814, #21328, #11800, #3379, #18397 ),
 .UNSPECIFIED., .F., .T. ) 
 B_SPLINE_CURVE_WITH_KNOTS ( ( 3, 2, 2, 2, 2, 2, 2, 2, 3 ),
 ( 0.06250000000000005551, 0.06445312500000009714, 0.06640625000000015266, 0.06835937500000019429, 0.07031250000000024980, 0.07226562500000029143, 0.07421875000000033307, 0.07617187500000038858, 0.07812500000000043021 ),
 .UNSPECIFIED. ) 
 CURVE ( )  GEOMETRIC_REPRESENTATION_ITEM ( )  RATIONAL_B_SPLINE_CURVE ( ( 0.9999999999999994449, 0.9807852804032309857, 1.000000000000000000, 0.9807852804032304306, 1.000000000000000000, 0.9807852804032304306, 1.000000000000000000, 0.9807852804032304306, 1.000000000000000000, 0.9807852804032304306, 1.000000000000000000, 0.9807852804032304306, 1.000000000000000000, 0.9807852804032304306, 1.000000000000000000, 0.9807852804032262117, 1.000000000000004219 ) ) 
 REPRESENTATION_ITEM ( '' )  );
#8044 = CARTESIAN_POINT ( 'NONE',  ( -28.68588794268869790, 222.8698905683720284, -16.75240474999999307 ) ) ;
#8045 = ORIENTED_EDGE ( 'NONE', *, *, #5512, .F. ) ;
#8046 = DIRECTION ( 'NONE',  ( -1.000000000000000000, 0.000000000000000000, 0.000000000000000000 ) ) ;
#8047 = ORIENTED_EDGE ( 'NONE', *, *, #14360, .F. ) ;
#8048 = CARTESIAN_POINT ( 'NONE',  ( -40.53162694259545162, 456.6198905683720568, 11.84573899990672885 ) ) ;
#8049 = CARTESIAN_POINT ( 'NONE',  ( -28.68588794268869435, 224.4948905765656377, 19.99999999999999289 ) ) ;
#8050 = AXIS2_PLACEMENT_3D ( 'NONE', #16559, #10254, #18162 ) ;
#8051 = ORIENTED_EDGE ( 'NONE', *, *, #4123, .F. ) ;
#8052 = CARTESIAN_POINT ( 'NONE',  ( -48.68588794268873698, 573.2448905601785327, 0.000000000000000000 ) ) ;
#8053 = CARTESIAN_POINT ( 'NONE',  ( -25.35362745456400191, 528.1823905683719431, 16.75240474999998952 ) ) ;
#8054 = CIRCLE ( 'NONE', #17732, 175.0000000000000284 ) ;
#8055 = ORIENTED_EDGE ( 'NONE', *, *, #13252, .F. ) ;
#8056 = CARTESIAN_POINT ( 'NONE',  ( -25.35362745456400901, 511.0573905683718863, -16.75240474999999307 ) ) ;
#8057 = CYLINDRICAL_SURFACE ( 'NONE', #7957, 21.20245194746112105 ) ;
#8058 = CARTESIAN_POINT ( 'NONE',  ( -45.64106924314020119, 451.0573905765656377, -11.32908994701042715 ) ) ;
#8059 = CARTESIAN_POINT ( 'NONE',  ( 4.700000000000000178, 0.000000000000000000, 0.000000000000000000 ) ) ;
#8060 = LINE ( 'NONE', #9792, #19597 ) ;
#8061 = LINE ( 'NONE', #6439, #9772 ) ;
#8062 = CARTESIAN_POINT ( 'NONE',  ( -11.73070664223723547, 237.9323905765656093, -11.32908994701042538 ) ) ;
#8063 = CARTESIAN_POINT ( 'NONE',  ( 20.42502041961814641, 160.1716627696692683, 60.00000000000000000 ) ) ;
#8064 =( NAMED_UNIT ( * ) PLANE_ANGLE_UNIT ( ) SI_UNIT ( $, .RADIAN. ) );
#8065 = CARTESIAN_POINT ( 'NONE',  ( -32.01814843081343298, 231.6823905683720568, -16.75240474999999307 ) ) ;
#8066 = CARTESIAN_POINT ( 'NONE',  ( -44.16309181155855867, 315.9948905683720568, 6.410867750099241924 ) ) ;
#8067 = CARTESIAN_POINT ( 'NONE',  ( 5.299999999999999822, -3.752776749732576356, -6.499999999999999112 ) ) ;
#8068 = CARTESIAN_POINT ( 'NONE',  ( -8.685887942688712116, 271.9323905601785327, 3.978247347593161010 ) ) ;
#8069 = CARTESIAN_POINT ( 'NONE',  ( -33.84809828339280102, 56.85652257517428865, -49.33155846391706945 ) ) ;
#8070 = CARTESIAN_POINT ( 'NONE',  ( -40.53162694259543031, 316.6198905683720568, 11.84573899990672885 ) ) ;
#8071 = EDGE_CURVE ( 'NONE', #11409, #15181, #20634, .T. ) ;
#8072 = CARTESIAN_POINT ( 'NONE',  ( -32.01814843081346140, 517.5573905683720568, 16.75240474999999307 ) ) ;
#8073 = CARTESIAN_POINT ( 'NONE',  ( -8.685887942688722774, 362.2448905601784190, -2.449293598294705724E-15 ) ) ;
#8074 = CARTESIAN_POINT ( 'NONE',  ( -42.82802356641965247, 315.9948905601784759, -14.14213562373094746 ) ) ;
#8075 = ORIENTED_EDGE ( 'NONE', *, *, #18160, .T. ) ;
#8076 = CARTESIAN_POINT ( 'NONE',  ( -28.68588794268872633, 477.8698905683720568, 16.75240474999999307 ) ) ;
#8077 = EDGE_CURVE ( 'NONE', #3125, #3575, #3741, .T. ) ;
#8078 = DIRECTION ( 'NONE',  ( -1.000000000000000000, 0.000000000000000000, 0.000000000000000000 ) ) ;
#8079 = CARTESIAN_POINT ( 'NONE',  ( -35.09675569278793716, 271.9948905683720000, -15.47720386886985544 ) ) ;
#8080 = ORIENTED_EDGE ( 'NONE', *, *, #10844, .F. ) ;
#8081 = CARTESIAN_POINT ( 'NONE',  ( -19.19641293061497578, 291.9323905683720568, -14.20200298773971603 ) ) ;
#8082 = CARTESIAN_POINT ( 'NONE',  ( -40.53162694259543031, 312.6198905683720000, -11.84573899990672707 ) ) ;
#8083 = CARTESIAN_POINT ( 'NONE',  ( -45.64106924314017988, 272.9323905765655809, 11.32908994701042715 ) ) ;
#8084 = DIRECTION ( 'NONE',  ( -0.000000000000000000, -0.000000000000000000, 1.000000000000000000 ) ) ;
#8085 = CARTESIAN_POINT ( 'NONE',  ( -18.68588794268873698, 323.8848358243226357, 20.00000000000000355 ) ) ;
#8086 = CARTESIAN_POINT ( 'NONE',  ( -44.16309181155857289, 374.7448905683720568, -6.410867750099231266 ) ) ;
#8087 = LINE ( 'NONE', #4966, #7508 ) ;
#8088 = CARTESIAN_POINT ( 'NONE',  ( 5.700000000000000178, 0.000000000000000000, 0.000000000000000000 ) ) ;
#8089 = EDGE_CURVE ( 'NONE', #19525, #21185, #16334, .T. ) ;
#8090 = ADVANCED_FACE ( 'NONE', ( #6022, #10883 ), #20955, .F. ) ;
#8091 = CARTESIAN_POINT ( 'NONE',  ( -22.27502019258948351, 426.9948905683720568, 15.47720386886985189 ) ) ;
#8092 = UNCERTAINTY_MEASURE_WITH_UNIT (LENGTH_MEASURE( 1.000000000000000082E-05 ), #20718, 'distance_accuracy_value', 'NONE');
#8093 = CARTESIAN_POINT ( 'NONE',  ( -28.68588794268874054, 573.2448905601785327, 0.000000000000000000 ) ) ;
#8094 = ORIENTED_EDGE ( 'NONE', *, *, #3408, .F. ) ;
#8095 = CARTESIAN_POINT ( 'NONE',  ( -14.54375231895777709, 423.4948905601784759, -14.14213562373094746 ) ) ;
#8096 = ORIENTED_EDGE ( 'NONE', *, *, #12661, .T. ) ;
#8097 = VERTEX_POINT ( 'NONE', #19118 ) ;
#8098 = CARTESIAN_POINT ( 'NONE',  ( -17.35679799567828852, 355.4323905765656377, 16.95518130045146421 ) ) ;
#8099 = CARTESIAN_POINT ( 'NONE',  ( -36.33955658999050087, 315.3698905601784759, -18.47759065022572855 ) ) ;
#8100 = CARTESIAN_POINT ( 'NONE',  ( -42.82802356641963826, 205.4725094246604442, -5.000000000000000888 ) ) ;
#8101 = CARTESIAN_POINT ( 'NONE',  ( -14.48388495494899786, 351.3073905683720568, -9.489475012073734561 ) ) ;
#8102 = CARTESIAN_POINT ( 'NONE',  ( -32.66413529028189799, 504.1823905765656946, 19.99999999999999289 ) ) ;
#8103 = CARTESIAN_POINT ( 'NONE',  ( -22.27502019258947996, 376.9948905683720568, 15.47720386886985189 ) ) ;
#8104 = CARTESIAN_POINT ( 'NONE',  ( -48.68588794268853803, 311.6823905765655809, -3.978247347593583783 ) ) ;
#8105 = CARTESIAN_POINT ( 'NONE',  ( -42.88789093042844058, 394.8073905683720000, 9.489475012073734561 ) ) ;
#8106 = ADVANCED_FACE ( 'NONE', ( #2789 ), #19003, .T. ) ;
#8107 = CARTESIAN_POINT ( 'NONE',  ( -17.35679799567829562, 318.5573905765656377, -16.95518130045146421 ) ) ;
#8108 = CARTESIAN_POINT ( 'NONE',  ( 27.98965548446208729, 333.8848358243226357, 40.00000000000000000 ) ) ;
#8109 = CARTESIAN_POINT ( 'NONE',  ( -42.88789093042842637, 292.9323905683720568, -9.489475012073734561 ) ) ;
#8110 = PLANE ( 'NONE',  #1512 ) ;
#8111 = CARTESIAN_POINT ( 'NONE',  ( -22.27502019258949417, 432.2448905683720000, -15.47720386886985544 ) ) ;
#8112 = CARTESIAN_POINT ( 'NONE',  ( -33.77147056149369320, 55.32675751745503590, 120.3516180215634819 ) ) ;
#8113 = LINE ( 'NONE', #19917, #16628 ) ;
#8114 = DIRECTION ( 'NONE',  ( 0.000000000000000000, -1.000000000000000000, 0.000000000000000000 ) ) ;
#8115 = CARTESIAN_POINT ( 'NONE',  ( -48.68588794268870146, 317.2448905601784759, 0.000000000000000000 ) ) ;
#8116 = EDGE_CURVE ( 'NONE', #17381, #3413, #12411, .T. ) ;
#8117 = CARTESIAN_POINT ( 'NONE',  ( -11.93348319268872260, 350.6823905683720000, -3.332260488124732856 ) ) ;
#8118 = CARTESIAN_POINT ( 'NONE',  ( -19.19641293061500065, 490.4323905683720000, -14.20200298773971603 ) ) ;
#8119 = ORIENTED_EDGE ( 'NONE', *, *, #15447, .T. ) ;
#8120 = CARTESIAN_POINT ( 'NONE',  ( -40.01497788969915348, 495.6823905601784759, -16.95518130045146421 ) ) ;
#8121 = CARTESIAN_POINT ( 'NONE',  ( -22.27502019258947996, 310.7448905683720000, -15.47720386886985544 ) ) ;
#8122 = ORIENTED_EDGE ( 'NONE', *, *, #6050, .F. ) ;
#8123 = CARTESIAN_POINT ( 'NONE',  ( 0.01372220897661549643, 5.309964801958114045, -3.802871176606129833 ) ) ;
#8124 = EDGE_LOOP ( 'NONE', ( #2355, #4443, #2988, #7336 ) ) ;
#8125 = PLANE ( 'NONE',  #3258 ) ;
#8126 = CARTESIAN_POINT ( 'NONE',  ( -45.43829269268871940, 405.3698905683720000, 0.000000000000000000 ) ) ;
#8127 = DIRECTION ( 'NONE',  ( 0.000000000000000000, 0.000000000000000000, -1.000000000000000000 ) ) ;
#8128 = FACE_OUTER_BOUND ( 'NONE', #2254, .T. ) ;
#8129 = CARTESIAN_POINT ( 'NONE',  ( -44.16309181155857289, 444.4948905683720568, 6.410867750099241924 ) ) ;
#8130 = CARTESIAN_POINT ( 'NONE',  ( -28.68588794268872633, 441.3698905683720000, -16.75240474999999307 ) ) ;
#8131 = DIRECTION ( 'NONE',  ( 1.000000000000000000, 0.000000000000000000, 0.000000000000000000 ) ) ;
#8132 = CARTESIAN_POINT ( 'NONE',  ( -45.64106924314018698, 416.3073905601785327, -11.32908994701042538 ) ) ;
#8133 = CARTESIAN_POINT ( 'NONE',  ( -48.68588794268871567, 392.3073905765656377, 3.978247347593168115 ) ) ;
#8134 = CARTESIAN_POINT ( 'NONE',  ( -17.74392196230863661, 46.24441999140541526, 48.38146745362002576 ) ) ;
#8135 = CYLINDRICAL_SURFACE ( 'NONE', #11303, 19.99999999999999645 ) ;
#8136 = CARTESIAN_POINT ( 'NONE',  ( 4.700000000000000178, 0.000000000000000000, 0.000000000000000000 ) ) ;
#8137 = CARTESIAN_POINT ( 'NONE',  ( 4.700000000000000178, 3.752776749732563033, 6.500000000000000000 ) ) ;
#8138 = CARTESIAN_POINT ( 'NONE',  ( -16.84014894278200103, 489.1198905683720000, 11.84573899990672530 ) ) ;
#8139 = DIRECTION ( 'NONE',  ( 0.000000000000000000, 0.000000000000000000, 1.000000000000000000 ) ) ;
#8140 = FILL_AREA_STYLE ('',( #8252 ) ) ;
#8141 = CARTESIAN_POINT ( 'NONE',  ( -48.68588794268885067, 417.5573905601784759, 3.978247347592849259 ) ) ;
#8142 = VECTOR ( 'NONE', #1128, 1000.000000000000000 ) ;
#8143 = CARTESIAN_POINT ( 'NONE',  ( -19.19641293061498999, 411.9323905683720000, -14.20200298773971603 ) ) ;
#8144 = CARTESIAN_POINT ( 'NONE',  ( -28.68588794268870146, 264.4948905765656377, 19.99999999999999289 ) ) ;
#8145 = EDGE_CURVE ( 'NONE', #11996, #445, #6155, .T. ) ;
#8146 = CARTESIAN_POINT ( 'NONE',  ( -19.19641293061497223, 231.9323905683720000, -14.20200298773971603 ) ) ;
#8147 = EDGE_CURVE ( 'NONE', #9302, #1002, #12734, .T. ) ;
#8148 = CIRCLE ( 'NONE', #9883, 220.7252770684331438 ) ;
#8149 = EDGE_LOOP ( 'NONE', ( #6705, #7311, #11457, #7034 ) ) ;
#8150 = CARTESIAN_POINT ( 'NONE',  ( -28.68588794268871922, 424.4948905765656377, 19.99999999999999289 ) ) ;
#8151 = ORIENTED_EDGE ( 'NONE', *, *, #15576, .T. ) ;
#8152 = CARTESIAN_POINT ( 'NONE',  ( -45.43829269268871940, 435.6823905683720568, 3.332260488124734632 ) ) ;
#8153 = CARTESIAN_POINT ( 'NONE',  ( -48.68588794268869435, 221.6823905765656662, -3.978247347593158345 ) ) ;
#8154 = VERTEX_POINT ( 'NONE', #4189 ) ;
#8155 = CARTESIAN_POINT ( 'NONE',  ( -43.67497163690818240, 210.1113231631601082, 0.6580207156766563203 ) ) ;
#8156 = CARTESIAN_POINT ( 'NONE',  ( -25.35362745456396283, 226.6823905683720284, 16.75240474999998952 ) ) ;
#8157 = EDGE_LOOP ( 'NONE', ( #12484, #13501, #3881, #2648, #1958, #17513, #1007, #11245, #3886, #6323 ) ) ;
#8158 = CARTESIAN_POINT ( 'NONE',  ( -40.53162694259545162, 502.6198905683720568, -11.84573899990672707 ) ) ;
#8159 = DIRECTION ( 'NONE',  ( 1.191790137725560488E-16, -1.000000000000000000, -0.000000000000000000 ) ) ;
#8160 = VECTOR ( 'NONE', #8580, 1000.000000000000000 ) ;
#8161 = CARTESIAN_POINT ( 'NONE',  ( -17.35679799567830273, 445.4323905765656377, 16.95518130045146421 ) ) ;
#8162 = CARTESIAN_POINT ( 'NONE',  ( -14.54375231895776288, 298.2448905765656377, -14.14213562373094746 ) ) ;
#8163 = DIRECTION ( 'NONE',  ( 1.000000000000000000, 0.000000000000000000, 0.000000000000000000 ) ) ;
#8164 = CYLINDRICAL_SURFACE ( 'NONE', #1866, 4.000000000000000000 ) ;
#8165 = DIRECTION ( 'NONE',  ( 0.000000000000000000, -1.000000000000000000, 0.000000000000000000 ) ) ;
#8166 = CARTESIAN_POINT ( 'NONE',  ( -8.685887942688713892, 292.2448905601784759, -2.449293598294705724E-15 ) ) ;
#8167 = VECTOR ( 'NONE', #9874, 1000.000000000000114 ) ;
#8168 = CARTESIAN_POINT ( 'NONE',  ( -34.34829387991847227, 223.9102039777116886, 19.24951607415172461 ) ) ;
#8169 = DIRECTION ( 'NONE',  ( -0.000000000000000000, -1.000000000000000000, -0.000000000000000000 ) ) ;
#8170 = B_SPLINE_CURVE_WITH_KNOTS ( 'NONE', 3,
 ( #7610, #21033, #7823, #9242, #4159, #4590, #14026, #17261 ),
 .UNSPECIFIED., .F., .F.,
 ( 4, 2, 2, 4 ),
 ( 0.003797433802554452380, 0.004743183970586248299, 0.005688934138618042050, 0.007580434474681631285 ),
 .UNSPECIFIED. ) ;
#8171 =( BOUNDED_CURVE ( )  B_SPLINE_CURVE ( 3, ( #17283, #4982, #20314, #2468 ),
 .UNSPECIFIED., .F., .T. ) 
 B_SPLINE_CURVE_WITH_KNOTS ( ( 4, 4 ),
 ( 3.164427803482926738, 4.712388980384689674 ),
 .UNSPECIFIED. ) 
 CURVE ( )  GEOMETRIC_REPRESENTATION_ITEM ( )  RATIONAL_B_SPLINE_CURVE ( ( 1.000000000000000000, 0.8100893075783975883, 0.8100893075783975883, 1.000000000000000000 ) ) 
 REPRESENTATION_ITEM ( '' )  );
#8172 = CARTESIAN_POINT ( 'NONE',  ( -32.01814843081344009, 327.5573905683720568, 16.75240474999999307 ) ) ;
#8173 = LINE ( 'NONE', #1183, #1274 ) ;
#8174 = CARTESIAN_POINT ( 'NONE',  ( -36.33955658999050087, 269.1198905601784759, 18.47759065022572500 ) ) ;
#8175 = CARTESIAN_POINT ( 'NONE',  ( -8.685887942688717445, 322.2448905601784759, -2.449293598294705724E-15 ) ) ;
#8176 = CARTESIAN_POINT ( 'NONE',  ( -40.53162694259543031, 286.6198905683720000, 11.84573899990672885 ) ) ;
#8177 = CARTESIAN_POINT ( 'NONE',  ( -25.35362745456401257, 532.5573905683720568, -16.75240474999999307 ) ) ;
#8178 = CARTESIAN_POINT ( 'NONE',  ( -42.82802356641965957, 358.4948905601785327, 14.14213562373094923 ) ) ;
#8179 = VECTOR ( 'NONE', #18076, 1000.000000000000000 ) ;
#8180 = LINE ( 'NONE', #16534, #9089 ) ;
#8181 = EDGE_LOOP ( 'NONE', ( #3231, #871, #1526, #9066 ) ) ;
#8182 = CARTESIAN_POINT ( 'NONE',  ( -40.53162694259545162, 484.1198905683720000, -11.84573899990672707 ) ) ;
#8183 = DIRECTION ( 'NONE',  ( 1.000000000000000000, 1.250996701150283068E-16, -0.000000000000000000 ) ) ;
#8184 = CARTESIAN_POINT ( 'NONE',  ( -22.27502019258946575, 276.9948905683720000, 15.47720386886985189 ) ) ;
#8185 = ORIENTED_EDGE ( 'NONE', *, *, #7376, .F. ) ;
#8186 = LINE ( 'NONE', #11146, #19021 ) ;
#8187 = CARTESIAN_POINT ( 'NONE',  ( -45.43829269268870519, 275.0573905683720568, -3.332260488124726638 ) ) ;
#8188 = CARTESIAN_POINT ( 'NONE',  ( -45.43829269268869808, 265.0573905683720568, -3.332260488124726638 ) ) ;
#8189 = VECTOR ( 'NONE', #9402, 1000.000000000000000 ) ;
#8190 = CARTESIAN_POINT ( 'NONE',  ( -8.685887942688708563, 237.3073905765656662, -3.978247347593165895 ) ) ;
#8191 = CARTESIAN_POINT ( 'NONE',  ( -8.685887942688605534, 472.5573905601784759, -3.978247347592846594 ) ) ;
#8192 = CARTESIAN_POINT ( 'NONE',  ( -32.01814843081343298, 226.0573905683720568, 16.75240474999999307 ) ) ;
#8193 = CARTESIAN_POINT ( 'NONE',  ( -32.01814843081343298, 266.0573905683720568, 16.75240474999999307 ) ) ;
#8194 = ADVANCED_FACE ( 'NONE', ( #11100 ), #16091, .T. ) ;
#8195 = CARTESIAN_POINT ( 'NONE',  ( -28.68588794268871922, 382.8698905683720000, -16.75240474999999307 ) ) ;
#8196 = AXIS2_PLACEMENT_3D ( 'NONE', #6365, #12974, #19565 ) ;
#8197 = CARTESIAN_POINT ( 'NONE',  ( 6.416697501590670427, 217.7548513357008630, -49.99999999999999289 ) ) ;
#8198 = CARTESIAN_POINT ( 'NONE',  ( -28.68588794268872988, 459.4948905765656377, -19.99999999999999289 ) ) ;
#8199 = PRODUCT_DEFINITION_SHAPE ( 'NONE', 'NONE',  #8621 ) ;
#8200 = ADVANCED_FACE ( 'NONE', ( #2574 ), #1270, .T. ) ;
#8201 = CARTESIAN_POINT ( 'NONE',  ( -49.57497958038185715, 160.1716627696692683, 50.00000000000000000 ) ) ;
#8202 = CARTESIAN_POINT ( 'NONE',  ( -32.01814843081345430, 426.0573905683720568, 16.75240474999999307 ) ) ;
#8203 = DIRECTION ( 'NONE',  ( -1.191790137725560488E-16, 1.000000000000000000, -0.000000000000000000 ) ) ;
#8204 = ORIENTED_EDGE ( 'NONE', *, *, #3927, .F. ) ;
#8205 = CARTESIAN_POINT ( 'NONE',  ( -40.01497788969913927, 418.8073905601785896, 16.95518130045146776 ) ) ;
#8206 = ORIENTED_EDGE ( 'NONE', *, *, #3716, .T. ) ;
#8207 = LINE ( 'NONE', #9938, #4946 ) ;
#8208 = ORIENTED_EDGE ( 'NONE', *, *, #17543, .T. ) ;
#8209 = EDGE_LOOP ( 'NONE', ( #17696, #10470, #16403, #6996 ) ) ;
#8210 = CARTESIAN_POINT ( 'NONE',  ( -24.70764059509554755, 354.8073905765656377, 19.99999999999998934 ) ) ;
#8211 = CARTESIAN_POINT ( 'NONE',  ( -11.73070664223724258, 303.1823905601784759, -11.32908994701042715 ) ) ;
#8212 = CARTESIAN_POINT ( 'NONE',  ( -43.68588794268873698, 548.2448905601784190, 1.836970198721029194E-15 ) ) ;
#8213 = CARTESIAN_POINT ( 'NONE',  ( -42.88789093042843348, 334.4323905683721136, -9.489475012073734561 ) ) ;
#8214 = CARTESIAN_POINT ( 'NONE',  ( -28.68588794268872988, 479.4948905765656377, -19.99999999999999289 ) ) ;
#8215 = CARTESIAN_POINT ( 'NONE',  ( -11.93348319268872260, 368.8698905683720000, -2.051577885510841163E-15 ) ) ;
#8216 = CARTESIAN_POINT ( 'NONE',  ( -40.01497788969913216, 310.4323905765656377, -16.95518130045146421 ) ) ;
#8217 = CARTESIAN_POINT ( 'NONE',  ( -38.17536295476246266, 392.3073905683720568, -14.20200298773971426 ) ) ;
#8218 = EDGE_CURVE ( 'NONE', #7167, #1107, #7216, .T. ) ;
#8219 = CARTESIAN_POINT ( 'NONE',  ( -47.16347859291443712, 311.3698905765656377, -7.653668647301793193 ) ) ;
#8220 = DIRECTION ( 'NONE',  ( -1.000000000000000000, -0.000000000000000000, -0.000000000000000000 ) ) ;
#8221 = CARTESIAN_POINT ( 'NONE',  ( -40.53162694259543031, 295.1198905683720000, 11.84573899990672885 ) ) ;
#8222 = FACE_OUTER_BOUND ( 'NONE', #9416, .T. ) ;
#8223 = CARTESIAN_POINT ( 'NONE',  ( -42.88789093042844058, 434.4323905683720568, -9.489475012073736337 ) ) ;
#8224 = AXIS2_PLACEMENT_3D ( 'NONE', #1323, #13104, #11359 ) ;
#8225 = CARTESIAN_POINT ( 'NONE',  ( 0.2595206531159287011, 2.531175536751829824, 6.499999999999999112 ) ) ;
#8226 = CARTESIAN_POINT ( 'NONE',  ( 107.6674317086782935, 187.4856410316723441, -20.00000000000000355 ) ) ;
#8227 = CARTESIAN_POINT ( 'NONE',  ( -47.16347859291445133, 447.8698905601785327, 7.653668647301805628 ) ) ;
#8228 = CARTESIAN_POINT ( 'NONE',  ( -42.88789093042843348, 344.4323905683720000, -9.489475012073736337 ) ) ;
#8229 = CARTESIAN_POINT ( 'NONE',  ( -38.17536295476246977, 492.3073905683720000, -14.20200298773971426 ) ) ;
#8230 = ORIENTED_EDGE ( 'NONE', *, *, #16371, .F. ) ;
#8231 = CARTESIAN_POINT ( 'NONE',  ( -28.68588794268873343, 494.7448905601785327, -19.99999999999999289 ) ) ;
#8232 = CARTESIAN_POINT ( 'NONE',  ( -35.09675569278793716, 311.9948905683720568, -15.47720386886985544 ) ) ;
#8233 = EDGE_CURVE ( 'NONE', #469, #12049, #15306, .T. ) ;
#8234 = ORIENTED_EDGE ( 'NONE', *, *, #13735, .T. ) ;
#8235 = CARTESIAN_POINT ( 'NONE',  ( -31.26501780185373391, 205.1437886375728965, 0.000000000000000000 ) ) ;
#8236 = ORIENTED_EDGE ( 'NONE', *, *, #15232, .F. ) ;
#8237 = PLANE ( 'NONE',  #10494 ) ;
#8238 = CARTESIAN_POINT ( 'NONE',  ( -44.16309181155857999, 404.7448905683720568, -6.410867750099231266 ) ) ;
#8239 = CARTESIAN_POINT ( 'NONE',  ( -48.68588794268870856, 377.2448905601784759, 0.000000000000000000 ) ) ;
#8240 = CARTESIAN_POINT ( 'NONE',  ( -40.53162694259544452, 422.6198905683720000, -11.84573899990672707 ) ) ;
#8241 = CARTESIAN_POINT ( 'NONE',  ( -16.84014894278200103, 450.1198905683720568, -11.84573899990672707 ) ) ;
#8242 = CONTEXT_DEPENDENT_SHAPE_REPRESENTATION ( #16074, #11312 ) ;
#8243 = CARTESIAN_POINT ( 'NONE',  ( -11.73070664223724968, 401.3073905601784190, 11.32908994701042005 ) ) ;
#8244 = EDGE_CURVE ( 'NONE', #7989, #9304, #16310, .T. ) ;
#8245 = CARTESIAN_POINT ( 'NONE',  ( -21.03221929538691271, 375.1198905765656377, 18.47759065022572500 ) ) ;
#8246 = CARTESIAN_POINT ( 'NONE',  ( -25.36425983038314058, 45.72515563955213480, 49.49023492600293395 ) ) ;
#8247 = DIRECTION ( 'NONE',  ( 0.000000000000000000, -0.000000000000000000, 1.000000000000000000 ) ) ;
#8248 = FACE_OUTER_BOUND ( 'NONE', #9939, .T. ) ;
#8249 = DIRECTION ( 'NONE',  ( 1.000000000000000000, -0.000000000000000000, -0.000000000000000000 ) ) ;
#8250 = CARTESIAN_POINT ( 'NONE',  ( -38.17536295476246977, 503.8073905683721136, -14.20200298773971426 ) ) ;
#8251 = DIRECTION ( 'NONE',  ( -1.000000000000000000, 0.000000000000000000, -0.000000000000000000 ) ) ;
#8252 = FILL_AREA_STYLE_COLOUR ( '', #19037 ) ;
#8253 = CARTESIAN_POINT ( 'NONE',  ( -28.68588794268872988, 519.7448905601784190, 19.99999999999999289 ) ) ;
#8254 = CIRCLE ( 'NONE', #16570, 4.000000000000000000 ) ;
#8255 = CARTESIAN_POINT ( 'NONE',  ( -42.88789093042844058, 404.4323905683721136, -9.489475012073736337 ) ) ;
#8256 = CARTESIAN_POINT ( 'NONE',  ( 20.42502041961813930, 230.5765313837437418, 40.00000000000000000 ) ) ;
#8257 = CARTESIAN_POINT ( 'NONE',  ( -42.88789093042841927, 224.4323905683720000, -9.489475012073736337 ) ) ;
#8258 = VERTEX_POINT ( 'NONE', #87 ) ;
#8259 = CARTESIAN_POINT ( 'NONE',  ( -48.68588794268871567, 421.9948905765656377, 0.000000000000000000 ) ) ;
#8260 = ORIENTED_EDGE ( 'NONE', *, *, #6761, .T. ) ;
#8261 = CARTESIAN_POINT ( 'NONE',  ( -40.53162694259544452, 434.1198905683720000, -11.84573899990672707 ) ) ;
#8262 = CARTESIAN_POINT ( 'NONE',  ( -13.20868407381887977, 528.2448905683720568, 6.410867750099229490 ) ) ;
#8263 = ORIENTED_EDGE ( 'NONE', *, *, #8780, .F. ) ;
#8264 = CARTESIAN_POINT ( 'NONE',  ( 20.42502041961814641, 160.1716627696692683, -60.00000000000000000 ) ) ;
#8265 = CARTESIAN_POINT ( 'NONE',  ( -28.68588794268873698, 532.8698905683719431, -16.75240474999999307 ) ) ;
#8266 = VERTEX_POINT ( 'NONE', #4715 ) ;
#8267 = CARTESIAN_POINT ( 'NONE',  ( -16.84014894278200813, 500.1198905683720000, -11.84573899990672707 ) ) ;
#8268 = CARTESIAN_POINT ( 'NONE',  ( -8.685887942688848895, 491.9323905601785327, 3.978247347593427907 ) ) ;
#8269 = AXIS2_PLACEMENT_3D ( 'NONE', #11032, #3830, #10419 ) ;
#8270 = CARTESIAN_POINT ( 'NONE',  ( -45.64106924314019409, 442.9323905765656377, 11.32908994701042715 ) ) ;
#8271 = CARTESIAN_POINT ( 'NONE',  ( 0.2565376335220200255, -2.516992571281979618, 6.500000000000000888 ) ) ;
#8272 = CARTESIAN_POINT ( 'NONE',  ( -21.03221929538690560, 330.3698905601784759, 18.47759065022572500 ) ) ;
#8273 = LINE ( 'NONE', #14797, #135 ) ;
#8274 = DIRECTION ( 'NONE',  ( 1.000000000000000000, 1.191790137725560488E-16, -1.178908271762451515E-16 ) ) ;
#8275 = EDGE_CURVE ( 'NONE', #15561, #12697, #11639, .T. ) ;
#8276 = FACE_OUTER_BOUND ( 'NONE', #7012, .T. ) ;
#8277 = CARTESIAN_POINT ( 'NONE',  ( 0.5805565836007642311, -3.752776749732576356, -6.499999999999999112 ) ) ;
#8278 = DIRECTION ( 'NONE',  ( 0.000000000000000000, 0.000000000000000000, 1.000000000000000000 ) ) ;
#8279 = CARTESIAN_POINT ( 'NONE',  ( -45.43829269268869808, 305.6823905683719431, 3.332260488124734632 ) ) ;
#8280 = DIRECTION ( 'NONE',  ( -0.000000000000000000, -0.000000000000000000, -1.000000000000000000 ) ) ;
#8281 = CARTESIAN_POINT ( 'NONE',  ( -10.20829729246297646, 272.8698905601784759, -7.653668647301794969 ) ) ;
#8282 = CARTESIAN_POINT ( 'NONE',  ( -47.16347859291445133, 412.6198905765656377, 7.653668647301805628 ) ) ;
#8283 = CARTESIAN_POINT ( 'NONE',  ( -22.27502019258947996, 292.2448905683720000, -15.47720386886985544 ) ) ;
#8284 = EDGE_CURVE ( 'NONE', #3359, #15417, #7544, .T. ) ;
#8285 = VECTOR ( 'NONE', #13250, 1000.000000000000000 ) ;
#8286 = CARTESIAN_POINT ( 'NONE',  ( -11.93348319268873858, 510.3698905683720000, -2.051577885510841163E-15 ) ) ;
#8287 = EDGE_CURVE ( 'NONE', #15817, #18169, #14795, .T. ) ;
#8288 = CARTESIAN_POINT ( 'NONE',  ( -21.03221929538692336, 374.1198905601785327, -18.47759065022572855 ) ) ;
#8289 = EDGE_CURVE ( 'NONE', #11027, #13749, #1955, .T. ) ;
#8290 = AXIS2_PLACEMENT_3D ( 'NONE', #532, #5269, #18670 ) ;
#8291 = CARTESIAN_POINT ( 'NONE',  ( -14.54375231895776466, 313.4948905601784759, -14.14213562373094746 ) ) ;
#8292 = VERTEX_POINT ( 'NONE', #3528 ) ;
#8293 = CARTESIAN_POINT ( 'NONE',  ( -19.19641293061499354, 461.9323905683720568, -14.20200298773971603 ) ) ;
#8294 = CARTESIAN_POINT ( 'NONE',  ( 147.4234352242185935, 610.7448905601785327, 1.893624729818134345 ) ) ;
#8295 = CARTESIAN_POINT ( 'NONE',  ( -38.17536295476244845, 272.3073905683720000, -14.20200298773971426 ) ) ;
#8296 = ORIENTED_EDGE ( 'NONE', *, *, #2966, .F. ) ;
#8297 = DIRECTION ( 'NONE',  ( 0.000000000000000000, 0.000000000000000000, 1.000000000000000000 ) ) ;
#8298 = CARTESIAN_POINT ( 'NONE',  ( -22.27502019258946575, 278.4948905683720000, 15.47720386886985189 ) ) ;
#8299 = CONICAL_SURFACE ( 'NONE', #6235, 6.500000000000000000, 1.047197551196600296 ) ;
#8300 = EDGE_CURVE ( 'NONE', #8848, #16774, #18538, .T. ) ;
#8301 = CARTESIAN_POINT ( 'NONE',  ( -42.82802356641964536, 240.7448905765656093, -14.14213562373094746 ) ) ;
#8302 = AXIS2_PLACEMENT_3D ( 'NONE', #18102, #16712, #3298 ) ;
#8303 = DIRECTION ( 'NONE',  ( 1.000000000000000000, 0.000000000000000000, 0.000000000000000000 ) ) ;
#8304 = CARTESIAN_POINT ( 'NONE',  ( -21.03221929538690560, 224.1198905601785043, -18.47759065022572855 ) ) ;
#8305 = DIRECTION ( 'NONE',  ( 1.000000000000000000, 0.000000000000000000, 0.000000000000000000 ) ) ;
#8306 = CARTESIAN_POINT ( 'NONE',  ( -45.43829269268869098, 263.5573905683720568, -3.332260488124726194 ) ) ;
#8307 = CARTESIAN_POINT ( 'NONE',  ( -14.48388495494899963, 369.4323905683720000, 9.489475012073732785 ) ) ;
#8308 = CARTESIAN_POINT ( 'NONE',  ( -43.20715004130836689, 201.8397834041948613, 3.766744768033092328 ) ) ;
#8309 = AXIS2_PLACEMENT_3D ( 'NONE', #5625, #12235, #6923 ) ;
#8310 = FACE_OUTER_BOUND ( 'NONE', #14677, .T. ) ;
#8311 = CARTESIAN_POINT ( 'NONE',  ( -22.27502019258948351, 416.9948905683720000, 15.47720386886985189 ) ) ;
#8312 = DIRECTION ( 'NONE',  ( 0.9365583756827543516, 0.000000000000000000, 0.3505116388060184329 ) ) ;
#8313 = VERTEX_POINT ( 'NONE', #16629 ) ;
#8314 = CARTESIAN_POINT ( 'NONE',  ( -47.16347859291445133, 426.6198905601785327, -7.653668647301793193 ) ) ;
#8315 = ORIENTED_EDGE ( 'NONE', *, *, #8145, .T. ) ;
#8316 = PRODUCT_DEFINITION_FORMATION_WITH_SPECIFIED_SOURCE ( 'ANY', '', #8019, .NOT_KNOWN. ) ;
#8317 = ORIENTED_EDGE ( 'NONE', *, *, #18289, .F. ) ;
#8318 = ORIENTED_EDGE ( 'NONE', *, *, #560, .T. ) ;
#8319 = CARTESIAN_POINT ( 'NONE',  ( -48.68588794268873698, 573.2448905601785327, 0.000000000000000000 ) ) ;
#8320 = CARTESIAN_POINT ( 'NONE',  ( -42.82802356641965247, 308.4948905601784759, 14.14213562373094923 ) ) ;
#8321 = LINE ( 'NONE', #9626, #10054 ) ;
#8322 = CARTESIAN_POINT ( 'NONE',  ( -35.09675569278794427, 353.4948905683720000, -15.47720386886985544 ) ) ;
#8323 = AXIS2_PLACEMENT_3D ( 'NONE', #3257, #16353, #9834 ) ;
#8324 = ORIENTED_EDGE ( 'NONE', *, *, #16321, .F. ) ;
#8325 = CARTESIAN_POINT ( 'NONE',  ( -10.20829729246300133, 487.6198905765656377, -7.653668647301794969 ) ) ;
#8326 = CARTESIAN_POINT ( 'NONE',  ( -16.84014894278198682, 367.6198905683720000, 11.84573899990672530 ) ) ;
#8327 = CARTESIAN_POINT ( 'NONE',  ( -40.53162694259544452, 395.1198905683720000, 11.84573899990672885 ) ) ;
#8328 = CARTESIAN_POINT ( 'NONE',  ( -42.82802356641965247, 313.2448905765656377, 14.14213562373094923 ) ) ;
#8329 = CYLINDRICAL_SURFACE ( 'NONE', #14166, 50.00000000000000000 ) ;
#8330 = CARTESIAN_POINT ( 'NONE',  ( -32.01814843081343298, 266.0573905683720568, 16.75240474999999307 ) ) ;
#8331 = CARTESIAN_POINT ( 'NONE',  ( -17.35679799567829917, 440.6823905601785327, 16.95518130045146421 ) ) ;
#8332 = CARTESIAN_POINT ( 'NONE',  ( -11.93348319268872970, 440.0573905683720000, 3.332260488124728415 ) ) ;
#8333 = CARTESIAN_POINT ( 'NONE',  ( -8.685887942688722774, 356.9948905765655809, -2.449293598294705724E-15 ) ) ;
#8334 = CARTESIAN_POINT ( 'NONE',  ( -8.685887942689104690, 501.9323905601783622, 3.978247347594039418 ) ) ;
#8335 = CYLINDRICAL_SURFACE ( 'NONE', #10912, 19.99999999999999645 ) ;
#8336 = PRODUCT_DEFINITION_CONTEXT ( 'detailed design', #7485, 'design' ) ;
#8337 = FACE_OUTER_BOUND ( 'NONE', #16454, .T. ) ;
#8338 = CARTESIAN_POINT ( 'NONE',  ( -14.48388495494899786, 341.3073905683720568, -9.489475012073736337 ) ) ;
#8339 = CARTESIAN_POINT ( 'NONE',  ( -32.01814843081346140, 491.6823905683720000, -16.75240474999999307 ) ) ;
#8340 = CONICAL_SURFACE ( 'NONE', #18011, 6.500000000000000000, 1.047197551196600296 ) ;
#8341 = ORIENTED_EDGE ( 'NONE', *, *, #19545, .T. ) ;
#8342 = CARTESIAN_POINT ( 'NONE',  ( -48.68588794268872277, 487.2448905601784759, 0.000000000000000000 ) ) ;
#8343 = CARTESIAN_POINT ( 'NONE',  ( -45.43829269268869808, 303.5573905683720568, -3.332260488124726194 ) ) ;
#8344 = EDGE_CURVE ( 'NONE', #14887, #19850, #10306, .T. ) ;
#8345 = CARTESIAN_POINT ( 'NONE',  ( 0.1061556211655345777, -4.836380039389415408, 4.623144047065558482 ) ) ;
#8346 = EDGE_LOOP ( 'NONE', ( #3693, #12704 ) ) ;
#8347 = PLANE ( 'NONE',  #7737 ) ;
#8348 = CARTESIAN_POINT ( 'NONE',  ( -25.35362745456399480, 402.5573905683720568, -16.75240474999999307 ) ) ;
#8349 = CARTESIAN_POINT ( 'NONE',  ( -45.64106924314017988, 376.3073905601784190, -11.32908994701042538 ) ) ;
#8350 = FACE_OUTER_BOUND ( 'NONE', #548, .T. ) ;
#8351 = CARTESIAN_POINT ( 'NONE',  ( -25.35362745456399836, 421.0573905683720000, -16.75240474999999307 ) ) ;
#8352 = CARTESIAN_POINT ( 'NONE',  ( -25.35362745456398059, 262.5573905683720000, -16.75240474999999307 ) ) ;
#8353 = CARTESIAN_POINT ( 'NONE',  ( -16.84014894278199748, 437.6198905683720000, 11.84573899990672530 ) ) ;
#8354 = SHAPE_DEFINITION_REPRESENTATION ( #9227, #1888 ) ;
#8355 = CARTESIAN_POINT ( 'NONE',  ( -71.26501780185373036, 130.1716627696692683, -25.00000000000000355 ) ) ;
#8356 = CARTESIAN_POINT ( 'NONE',  ( -8.685887942688720997, 356.6823905765656377, 3.978247347593161010 ) ) ;
#8357 = CARTESIAN_POINT ( 'NONE',  ( -162.2727221670389781, 10.52886280891152104, 0.000000000000000000 ) ) ;
#8358 = CARTESIAN_POINT ( 'NONE',  ( -10.20829729246297468, 262.8698905601785327, -7.653668647301794969 ) ) ;
#8359 = CARTESIAN_POINT ( 'NONE',  ( -42.82802356641966668, 430.7448905765656377, -14.14213562373094746 ) ) ;
#8360 = CARTESIAN_POINT ( 'NONE',  ( 91.21585410611801592, 56.85652257517428865, -94.99999999999994316 ) ) ;
#8361=STYLED_ITEM('',(#21442),#4508);
#8362 = CARTESIAN_POINT ( 'NONE',  ( -14.48388495494901562, 499.4323905683720000, 9.489475012073732785 ) ) ;
#8363 = EDGE_CURVE ( 'NONE', #6373, #18883, #13087, .T. ) ;
#8364 = DIRECTION ( 'NONE',  ( 0.000000000000000000, 1.000000000000000000, 0.000000000000000000 ) ) ;
#8365 = DIRECTION ( 'NONE',  ( -1.191790137725560488E-16, 1.000000000000000000, -0.000000000000000000 ) ) ;
#8366 = CARTESIAN_POINT ( 'NONE',  ( -21.03221929538691626, 420.3698905601784759, 18.47759065022572500 ) ) ;
#8367 = CARTESIAN_POINT ( 'NONE',  ( -16.84014894278199392, 409.1198905683720000, 11.84573899990672530 ) ) ;
#8368 = CARTESIAN_POINT ( 'NONE',  ( -32.66413529028185536, 264.1823905765656946, 19.99999999999999289 ) ) ;
#8369 = CIRCLE ( 'NONE', #14954, 20.00000000000000000 ) ;
#8370 = CARTESIAN_POINT ( 'NONE',  ( -40.53162694259542320, 226.6198905683720000, 11.84573899990672885 ) ) ;
#8371 = CARTESIAN_POINT ( 'NONE',  ( -22.27502019258947641, 366.9948905683720568, 15.47720386886985189 ) ) ;
#8372 = EDGE_CURVE ( 'NONE', #2086, #1584, #653, .T. ) ;
#8373 = ORIENTED_EDGE ( 'NONE', *, *, #14403, .T. ) ;
#8374 = CARTESIAN_POINT ( 'NONE',  ( -22.27502019258950483, 530.7448905683720568, -15.47720386886985544 ) ) ;
#8375 = ORIENTED_EDGE ( 'NONE', *, *, #15894, .F. ) ;
#8376 = CARTESIAN_POINT ( 'NONE',  ( -32.01814843081345430, 453.1823905683720568, -16.75240474999999307 ) ) ;
#8377 = CARTESIAN_POINT ( 'NONE',  ( -38.17536295476247687, 532.3073905683719431, -14.20200298773971426 ) ) ;
#8378 = ORIENTED_EDGE ( 'NONE', *, *, #14669, .T. ) ;
#8379 = CARTESIAN_POINT ( 'NONE',  ( -48.68588794268872988, 531.6823905765655809, -3.978247347593157901 ) ) ;
#8380 = CARTESIAN_POINT ( 'NONE',  ( -16.84014894278200458, 490.1198905683720000, -11.84573899990672707 ) ) ;
#8381 = VERTEX_POINT ( 'NONE', #21164 ) ;
#8382 = CARTESIAN_POINT ( 'NONE',  ( -16.84014894278200813, 510.1198905683720568, -11.84573899990672707 ) ) ;
#8383 = CARTESIAN_POINT ( 'NONE',  ( -11.91940135186754723, 51.80353952486193947, -46.68172999105591714 ) ) ;
#8384 = CARTESIAN_POINT ( 'NONE',  ( -10.20829729246299422, 427.6198905765656377, -7.653668647301794969 ) ) ;
#8385 = CARTESIAN_POINT ( 'NONE',  ( -48.68588794268870856, 361.9948905765655809, 0.000000000000000000 ) ) ;
#8386 = CARTESIAN_POINT ( 'NONE',  ( -47.16347859291443001, 251.3698905765656093, -7.653668647301793193 ) ) ;
#8387 = DIRECTION ( 'NONE',  ( 0.000000000000000000, 0.000000000000000000, 1.000000000000000000 ) ) ;
#8388 = DIRECTION ( 'NONE',  ( 0.000000000000000000, -0.000000000000000000, 1.000000000000000000 ) ) ;
#8389 = CARTESIAN_POINT ( 'NONE',  ( -71.26501780185373036, 326.0737056351150613, 0.000000000000000000 ) ) ;
#8390 = CIRCLE ( 'NONE', #20487, 10.00000000000000888 ) ;
#8391 = CYLINDRICAL_SURFACE ( 'NONE', #20109, 19.99999999999999645 ) ;
#8392 = CARTESIAN_POINT ( 'NONE',  ( -8.685887942688703234, 223.9102039777117170, -1.743609257155848136 ) ) ;
#8393 = CARTESIAN_POINT ( 'NONE',  ( -44.16309181155855867, 295.9948905683720000, 6.410867750099241924 ) ) ;
#8394 = CARTESIAN_POINT ( 'NONE',  ( -8.685887942688742314, 532.2448905601784190, -2.449293598294705724E-15 ) ) ;
#8395 = CARTESIAN_POINT ( 'NONE',  ( -40.01497788969912506, 278.8073905601785327, 16.95518130045146776 ) ) ;
#8396 = CARTESIAN_POINT ( 'NONE',  ( -30.52044739588059841, 48.73524092274013242, -49.56800486934177741 ) ) ;
#8397 = CARTESIAN_POINT ( 'NONE',  ( -44.16309181155856578, 284.7448905683720568, -6.410867750099231266 ) ) ;
#8398 = VECTOR ( 'NONE', #15820, 1000.000000000000000 ) ;
#8399 = LINE ( 'NONE', #20197, #2907 ) ;
#8400 = CARTESIAN_POINT ( 'NONE',  ( -22.27502019258950128, 512.2448905683720568, -15.47720386886985544 ) ) ;
#8401 = CIRCLE ( 'NONE', #3910, 4.000000000000001776 ) ;
#8402 = DIRECTION ( 'NONE',  ( 0.000000000000000000, 0.000000000000000000, 1.000000000000000000 ) ) ;
#8403 = ORIENTED_EDGE ( 'NONE', *, *, #19133, .F. ) ;
#8404 = CARTESIAN_POINT ( 'NONE',  ( -45.43829269268871940, 475.0573905683720000, -3.332260488124726194 ) ) ;
#8405 = B_SPLINE_CURVE_WITH_KNOTS ( 'NONE', 3,
 ( #1529, #8100, #14729, #6482, #3885, #5191, #20439, #18383, #18804, #16780, #11788, #7121, #16990, #237, #6806, #10259, #20123, #13534, #3572, #660 ),
 .UNSPECIFIED., .F., .F.,
 ( 4, 2, 2, 2, 2, 2, 2, 2, 2, 4 ),
 ( 0.007875367097399143743, 0.008859169463295337929, 0.009842971829191532115, 0.01082677419508772804, 0.01181057656098392222, 0.01279437892688011641, 0.01377818129277631060, 0.01476198365867250478, 0.01525388484162060188, 0.01574578602456869897 ),
 .UNSPECIFIED. ) ;
#8406 = CARTESIAN_POINT ( 'NONE',  ( -48.68588794268858067, 411.6823905765655240, -3.978247347593477201 ) ) ;
#8407 = CARTESIAN_POINT ( 'NONE',  ( -32.01814843081343298, 266.0573905683720568, 16.75240474999999307 ) ) ;
#8408 = ORIENTED_EDGE ( 'NONE', *, *, #10736, .F. ) ;
#8409 = CARTESIAN_POINT ( 'NONE',  ( -14.54375231895776466, 335.7448905765655809, 14.14213562373094568 ) ) ;
#8410 = CARTESIAN_POINT ( 'NONE',  ( -45.43829269268869808, 235.0573905683720568, -3.332260488124726638 ) ) ;
#8411 = CIRCLE ( 'NONE', #1878, 4.000000000000003553 ) ;
#8412 = CARTESIAN_POINT ( 'NONE',  ( -10.20829729246297291, 246.3698905765656093, 7.653668647301790529 ) ) ;
#8413 = CARTESIAN_POINT ( 'NONE',  ( 15.48595089668572555, 220.7569358267784025, 2.447515658234522107 ) ) ;
#8414 = CARTESIAN_POINT ( 'NONE',  ( -6.276925316985663805, 600.7448905601785327, 44.69718552705352010 ) ) ;
#8415 = CARTESIAN_POINT ( 'NONE',  ( -19.19641293061497578, 260.4323905683720000, -14.20200298773971603 ) ) ;
#8416 = EDGE_CURVE ( 'NONE', #12168, #4317, #15527, .T. ) ;
#8417 = VECTOR ( 'NONE', #3108, 1000.000000000000000 ) ;
#8418 = CARTESIAN_POINT ( 'NONE',  ( -45.43829269268870519, 365.0573905683720568, -3.332260488124726194 ) ) ;
#8419 = CARTESIAN_POINT ( 'NONE',  ( -28.68588794268872633, 333.8848358243226357, -38.00000000000000000 ) ) ;
#8420 = DIRECTION ( 'NONE',  ( 1.000000000000000000, 0.000000000000000000, -0.000000000000000000 ) ) ;
#8421 = CARTESIAN_POINT ( 'NONE',  ( -28.68588794268871922, 416.3698905683720568, 16.75240474999999307 ) ) ;
#8422 = CARTESIAN_POINT ( 'NONE',  ( -32.66413529028186957, 339.8073905765656377, -19.99999999999999289 ) ) ;
#8423 = VERTEX_POINT ( 'NONE', #13915 ) ;
#8424 = CARTESIAN_POINT ( 'NONE',  ( -42.82802356641966668, 408.4948905601784759, 14.14213562373094923 ) ) ;
#8425 = ADVANCED_FACE ( 'NONE', ( #1925 ), #3634, .F. ) ;
#8426 = VERTEX_POINT ( 'NONE', #8595 ) ;
#8427 = DIRECTION ( 'NONE',  ( -0.000000000000000000, -1.000000000000000000, -0.000000000000000000 ) ) ;
#8428 = ORIENTED_EDGE ( 'NONE', *, *, #717, .T. ) ;
#8429 = CARTESIAN_POINT ( 'NONE',  ( -40.53162694259545873, 534.1198905683720568, -11.84573899990672707 ) ) ;
#8430 = CARTESIAN_POINT ( 'NONE',  ( -45.64106924314017988, 306.3073905601784190, -11.32908994701042715 ) ) ;
#8431 = CARTESIAN_POINT ( 'NONE',  ( 4.700000000000000178, 0.000000000000000000, -6.500000000000000000 ) ) ;
#8432 = ORIENTED_EDGE ( 'NONE', *, *, #4061, .F. ) ;
#8433 =( BOUNDED_CURVE ( )  B_SPLINE_CURVE ( 2, ( #17775, #14543, #12806, #12914, #21129, #17980, #4683, #1140, #3068, #11173, #1342, #7599, #6087, #9652, #21237, #9759, #4582 ),
 .UNSPECIFIED., .F., .T. ) 
 B_SPLINE_CURVE_WITH_KNOTS ( ( 3, 2, 2, 2, 2, 2, 2, 2, 3 ),
 ( 0.9218750000000001110, 0.9238281250000001110, 0.9257812500000001110, 0.9277343750000001110, 0.9296875000000001110, 0.9316406250000001110, 0.9335937500000001110, 0.9355468750000001110, 0.9375000000000001110 ),
 .UNSPECIFIED. ) 
 CURVE ( )  GEOMETRIC_REPRESENTATION_ITEM ( )  RATIONAL_B_SPLINE_CURVE ( ( 0.9999999999999988898, 0.9807852804032315408, 1.000000000000000000, 0.9807852804032304306, 1.000000000000000000, 0.9807852804032304306, 1.000000000000000000, 0.9807852804032304306, 1.000000000000000000, 0.9807852804032304306, 1.000000000000000000, 0.9807852804032304306, 1.000000000000000000, 0.9807852804032304306, 1.000000000000000000, 0.9807852804032293204, 1.000000000000001110 ) ) 
 REPRESENTATION_ITEM ( '' )  );
#8434 = VECTOR ( 'NONE', #12912, 1000.000000000000000 ) ;
#8435 = CARTESIAN_POINT ( 'NONE',  ( -16.84014894278198682, 321.6198905683720568, -11.84573899990672707 ) ) ;
#8436 = CARTESIAN_POINT ( 'NONE',  ( -32.01814843081344719, 356.0573905683719431, 16.75240474999999307 ) ) ;
#8437 = CARTESIAN_POINT ( 'NONE',  ( -16.84014894278199037, 360.1198905683720000, -11.84573899990672707 ) ) ;
#8438 = CARTESIAN_POINT ( 'NONE',  ( -45.64106924314017988, 302.9323905765655809, 11.32908994701042715 ) ) ;
#8439 = DIRECTION ( 'NONE',  ( 0.000000000000000000, 0.000000000000000000, 1.000000000000000000 ) ) ;
#8440 = CARTESIAN_POINT ( 'NONE',  ( -42.88789093042842637, 274.8073905683720000, 9.489475012073734561 ) ) ;
#8441 = CARTESIAN_POINT ( 'NONE',  ( -40.01497788969913927, 438.8073905601784190, 16.95518130045146776 ) ) ;
#8442 = CARTESIAN_POINT ( 'NONE',  ( -42.88789093042844058, 426.3073905683720568, 9.489475012073736337 ) ) ;
#8443 = CARTESIAN_POINT ( 'NONE',  ( -28.68588794268874054, 573.2448905601785327, 0.000000000000000000 ) ) ;
#8444 = CARTESIAN_POINT ( 'NONE',  ( -32.66413529028189089, 515.0573905601785327, -19.99999999999999289 ) ) ;
#8445 = CARTESIAN_POINT ( 'NONE',  ( -8.685887942688742314, 573.2448905601785327, 2.449293598294706119E-15 ) ) ;
#8446 = DIRECTION ( 'NONE',  ( 0.000000000000000000, -1.000000000000000000, 0.000000000000000000 ) ) ;
#8447 = CARTESIAN_POINT ( 'NONE',  ( -25.35362745456397704, 328.1823905683720568, 16.75240474999998952 ) ) ;
#8448 = CARTESIAN_POINT ( 'NONE',  ( -14.48388495494901029, 477.9323905683721136, 9.489475012073732785 ) ) ;
#8449 = ORIENTED_EDGE ( 'NONE', *, *, #5505, .F. ) ;
#8450 = CARTESIAN_POINT ( 'NONE',  ( -40.01497788969914637, 478.8073905601784759, 16.95518130045146776 ) ) ;
#8451 = CARTESIAN_POINT ( 'NONE',  ( -35.09675569278793716, 301.9948905683720568, -15.47720386886985544 ) ) ;
#8452 = ORIENTED_EDGE ( 'NONE', *, *, #17251, .F. ) ;
#8453 = CARTESIAN_POINT ( 'NONE',  ( 0.2578475836320701653, -4.367703157927325996, 5.434916218090832807 ) ) ;
#8454 = ORIENTED_EDGE ( 'NONE', *, *, #9819, .F. ) ;
#8455 = DIRECTION ( 'NONE',  ( 0.000000000000000000, 0.000000000000000000, 1.000000000000000000 ) ) ;
#8456 = CARTESIAN_POINT ( 'NONE',  ( -32.01814843081344719, 413.1823905683719431, -16.75240474999999307 ) ) ;
#8457 = CARTESIAN_POINT ( 'NONE',  ( -8.685887942688868435, 481.9323905601784759, 3.978247347593479866 ) ) ;
#8458 = CARTESIAN_POINT ( 'NONE',  ( -45.64106924314017988, 382.9323905765656377, 11.32908994701042538 ) ) ;
#8459 = CARTESIAN_POINT ( 'NONE',  ( -19.19641293061498999, 417.3073905683720568, 14.20200298773971426 ) ) ;
#8460 = CARTESIAN_POINT ( 'NONE',  ( -45.43829269268869808, 265.3698905683720000, 0.000000000000000000 ) ) ;
#8461 = CARTESIAN_POINT ( 'NONE',  ( -40.53162694259544452, 422.6198905683720000, -11.84573899990672707 ) ) ;
#8462 = SHAPE_DEFINITION_REPRESENTATION ( #21163, #8616 ) ;
#8463 = DIRECTION ( 'NONE',  ( -1.191790137725560488E-16, 1.000000000000000000, -0.000000000000000000 ) ) ;
#8464 = CIRCLE ( 'NONE', #2564, 4.000000000000001776 ) ;
#8465 = CARTESIAN_POINT ( 'NONE',  ( -32.66413529028187668, 359.8073905765656946, -19.99999999999999289 ) ) ;
#8466 = CARTESIAN_POINT ( 'NONE',  ( -8.685887942688712116, 272.2448905601784759, -2.449293598294705724E-15 ) ) ;
#8467 = CARTESIAN_POINT ( 'NONE',  ( 40.42502041961814996, 180.1716627696692967, -20.00000000000000355 ) ) ;
#8468 = CARTESIAN_POINT ( 'NONE',  ( -32.01814843081344719, 331.6823905683720000, -16.75240474999999307 ) ) ;
#8469 = FACE_OUTER_BOUND ( 'NONE', #7570, .T. ) ;
#8470 = CARTESIAN_POINT ( 'NONE',  ( -45.43829269268872650, 505.3698905683721136, 0.000000000000000000 ) ) ;
#8471 = EDGE_CURVE ( 'NONE', #1920, #16558, #15218, .T. ) ;
#8472 = DIRECTION ( 'NONE',  ( 0.000000000000000000, 0.000000000000000000, -1.000000000000000000 ) ) ;
#8473 = CARTESIAN_POINT ( 'NONE',  ( -8.685887942688742314, 573.2448905601785327, 2.449293598294706119E-15 ) ) ;
#8474 = CARTESIAN_POINT ( 'NONE',  ( -43.67243589781770652, 210.1033101532991338, 0.6559853996653204344 ) ) ;
#8475 = CARTESIAN_POINT ( 'NONE',  ( -35.09675569278795138, 387.2448905683720000, 15.47720386886985366 ) ) ;
#8476 = CARTESIAN_POINT ( 'NONE',  ( -21.03221929538693757, 468.8698905765656377, -18.47759065022572855 ) ) ;
#8477 = EDGE_CURVE ( 'NONE', #21185, #12399, #8924, .T. ) ;
#8478 = CARTESIAN_POINT ( 'NONE',  ( -32.01814843081343298, 227.5573905683720568, 16.75240474999999307 ) ) ;
#8479 = CARTESIAN_POINT ( 'NONE',  ( -13.20868407381886023, 368.2448905683720000, 6.410867750099229490 ) ) ;
#8480 = ORIENTED_EDGE ( 'NONE', *, *, #8950, .T. ) ;
#8481 = CARTESIAN_POINT ( 'NONE',  ( -38.17536295476246977, 515.4323905683720568, 14.20200298773971781 ) ) ;
#8482 = ORIENTED_EDGE ( 'NONE', *, *, #17293, .F. ) ;
#8483 = CARTESIAN_POINT ( 'NONE',  ( -32.01814843081344719, 437.5573905683720000, 16.75240474999999307 ) ) ;
#8484 = CARTESIAN_POINT ( 'NONE',  ( -22.27502019258950483, 530.7448905683720568, -15.47720386886985544 ) ) ;
#8485 = DIRECTION ( 'NONE',  ( -0.000000000000000000, -0.000000000000000000, -1.000000000000000000 ) ) ;
#8486 = CARTESIAN_POINT ( 'NONE',  ( 43.53705524234220547, 30.52886280891152282, -96.62835994548002816 ) ) ;
#8487 = CARTESIAN_POINT ( 'NONE',  ( -35.09675569278795848, 491.9948905683720568, -15.47720386886985544 ) ) ;
#8488 = ORIENTED_EDGE ( 'NONE', *, *, #16321, .T. ) ;
#8489 = CARTESIAN_POINT ( 'NONE',  ( -32.01814843081346140, 506.0573905683719431, 16.75240474999999307 ) ) ;
#8490 = CARTESIAN_POINT ( 'NONE',  ( -10.91048723079944871, 54.76430750887173105, -46.30741063304804328 ) ) ;
#8491 = CARTESIAN_POINT ( 'NONE',  ( -11.73070664223725501, 426.0573905765656377, 11.32908994701042005 ) ) ;
#8492 = DIRECTION ( 'NONE',  ( 0.000000000000000000, 0.000000000000000000, 1.000000000000000000 ) ) ;
#8493 = DIRECTION ( 'NONE',  ( 1.000000000000000000, 0.000000000000000000, 0.000000000000000000 ) ) ;
#8494 = CARTESIAN_POINT ( 'NONE',  ( -48.68588794268861619, 486.9323905601785896, -3.978247347593425243 ) ) ;
#8495 = CARTESIAN_POINT ( 'NONE',  ( 0.1061556211655389631, -6.421950209808288790, -1.876855952934453731 ) ) ;
#8496 =( BOUNDED_CURVE ( )  B_SPLINE_CURVE ( 2, ( #1599, #19759, #13172, #4942, #19440, #18132, #4624, #16002, #1824, #13391, #3537, #8500, #5469, #6665, #6877, #5359, #10015 ),
 .UNSPECIFIED., .F., .T. ) 
 B_SPLINE_CURVE_WITH_KNOTS ( ( 3, 2, 2, 2, 2, 2, 2, 2, 3 ),
 ( 0.9375000000000001110, 0.9394531250000001110, 0.9414062500000001110, 0.9433593750000001110, 0.9453125000000001110, 0.9472656250000001110, 0.9492187500000001110, 0.9511718750000001110, 0.9531250000000001110 ),
 .UNSPECIFIED. ) 
 CURVE ( )  GEOMETRIC_REPRESENTATION_ITEM ( )  RATIONAL_B_SPLINE_CURVE ( ( 0.9999999999999988898, 0.9807852804032315408, 1.000000000000000000, 0.9807852804032304306, 1.000000000000000000, 0.9807852804032304306, 1.000000000000000000, 0.9807852804032304306, 1.000000000000000000, 0.9807852804032304306, 1.000000000000000000, 0.9807852804032304306, 1.000000000000000000, 0.9807852804032304306, 1.000000000000000000, 0.9807852804032293204, 1.000000000000001110 ) ) 
 REPRESENTATION_ITEM ( '' )  );
#8497 = EDGE_CURVE ( 'NONE', #554, #739, #15864, .T. ) ;
#8498 = DIRECTION ( 'NONE',  ( -1.191790137725560488E-16, 1.000000000000000000, -0.000000000000000000 ) ) ;
#8499 = CARTESIAN_POINT ( 'NONE',  ( -25.35362745456398414, 302.5573905683720000, -16.75240474999999307 ) ) ;
#8500 = CARTESIAN_POINT ( 'NONE',  ( -17.35679799567828141, 233.8073905601784759, -16.95518130045146421 ) ) ;
#8501 = CARTESIAN_POINT ( 'NONE',  ( -17.35679799567828852, 263.8073905601784759, -16.95518130045146421 ) ) ;
#8502 = CARTESIAN_POINT ( 'NONE',  ( 35.96497763894178945, 230.5765313837437418, 60.00000000000000000 ) ) ;
#8503 = CARTESIAN_POINT ( 'NONE',  ( -16.84014894278198327, 291.6198905683720000, -11.84573899990672707 ) ) ;
#8504 = ORIENTED_EDGE ( 'NONE', *, *, #11734, .T. ) ;
#8505 = CARTESIAN_POINT ( 'NONE',  ( -14.54375231895775578, 270.9948905601784759, 14.14213562373094568 ) ) ;
#8506 = CARTESIAN_POINT ( 'NONE',  ( -45.43829269268872650, 505.0573905683720568, -3.332260488124726638 ) ) ;
#8507 = ADVANCED_FACE ( 'NONE', ( #3841 ), #5352, .F. ) ;
#8508 = CIRCLE ( 'NONE', #13700, 4.000000000000000000 ) ;
#8509 = ORIENTED_EDGE ( 'NONE', *, *, #11412, .T. ) ;
#8510 = CARTESIAN_POINT ( 'NONE',  ( -13.20868407381887089, 459.7448905683720568, 6.410867750099229490 ) ) ;
#8511 = CARTESIAN_POINT ( 'NONE',  ( -8.685887942688726326, 406.9948905765656377, -2.449293598294705724E-15 ) ) ;
#8512 = CARTESIAN_POINT ( 'NONE',  ( -16.84014894278197616, 257.6198905683720568, 11.84573899990672530 ) ) ;
#8513 = ORIENTED_EDGE ( 'NONE', *, *, #14518, .F. ) ;
#8514 = CARTESIAN_POINT ( 'NONE',  ( -42.82802356641965957, 333.2448905765656377, 14.14213562373094923 ) ) ;
#8515 = AXIS2_PLACEMENT_3D ( 'NONE', #15656, #10759, #15759 ) ;
#8516 = CARTESIAN_POINT ( 'NONE',  ( -22.27502019258946220, 238.4948905683720284, 15.47720386886985189 ) ) ;
#8517 = EDGE_CURVE ( 'NONE', #15103, #554, #16840, .T. ) ;
#8518 = CARTESIAN_POINT ( 'NONE',  ( -42.82802356641964536, 243.2448905765656093, 14.14213562373094923 ) ) ;
#8519 = CARTESIAN_POINT ( 'NONE',  ( 5.674999999999999822, 3.752776749732560368, -6.499999999999999112 ) ) ;
#8520 = CARTESIAN_POINT ( 'NONE',  ( -28.68588794268869435, 229.7448905601785043, 19.99999999999999289 ) ) ;
#8521 = CARTESIAN_POINT ( 'NONE',  ( -45.43829269268870519, 273.8698905683720000, 0.000000000000000000 ) ) ;
#8522 = CARTESIAN_POINT ( 'NONE',  ( -11.93348319268872260, 360.0573905683719431, 3.332260488124728415 ) ) ;
#8523 = AXIS2_PLACEMENT_3D ( 'NONE', #18243, #14912, #96 ) ;
#8524 = CARTESIAN_POINT ( 'NONE',  ( -21.03221929538694113, 504.1198905601784759, -18.47759065022572855 ) ) ;
#8525 = CIRCLE ( 'NONE', #14426, 21.20245194746113526 ) ;
#8526 = CARTESIAN_POINT ( 'NONE',  ( -40.53162694259544452, 395.1198905683720000, 11.84573899990672885 ) ) ;
#8527 = CARTESIAN_POINT ( 'NONE',  ( -14.54375231895776821, 338.2448905765656377, -14.14213562373094746 ) ) ;
#8528 = ORIENTED_EDGE ( 'NONE', *, *, #15056, .F. ) ;
#8529 = CARTESIAN_POINT ( 'NONE',  ( -48.68588794268871567, 406.9323905601784759, -3.978247347593158345 ) ) ;
#8530 = ORIENTED_EDGE ( 'NONE', *, *, #8497, .T. ) ;
#8531 = CARTESIAN_POINT ( 'NONE',  ( 0.2595206531159274244, 2.531175536751827160, -6.499999999999999112 ) ) ;
#8532 = ORIENTED_EDGE ( 'NONE', *, *, #2046, .T. ) ;
#8533 = ORIENTED_EDGE ( 'NONE', *, *, #14991, .T. ) ;
#8534 = CARTESIAN_POINT ( 'NONE',  ( -13.20868407381887977, 520.9948905683720568, -6.410867750099233042 ) ) ;
#8535 = CARTESIAN_POINT ( 'NONE',  ( -40.01497788969913216, 285.6823905601784759, -16.95518130045146421 ) ) ;
#8536 = CYLINDRICAL_SURFACE ( 'NONE', #1113, 25.00000000000000711 ) ;
#8537 = EDGE_LOOP ( 'NONE', ( #16449, #20949, #10047, #16349 ) ) ;
#8538 = CARTESIAN_POINT ( 'NONE',  ( -38.17536295476244135, 326.9323905683720568, 14.20200298773971781 ) ) ;
#8539 = VECTOR ( 'NONE', #12174, 1000.000000000000000 ) ;
#8540 = CARTESIAN_POINT ( 'NONE',  ( -11.93348319268872082, 358.8698905683720000, -2.051577885510841163E-15 ) ) ;
#8541 = CARTESIAN_POINT ( 'NONE',  ( -11.93348319268872260, 369.1823905683720000, -3.332260488124732856 ) ) ;
#8542 = AXIS2_PLACEMENT_3D ( 'NONE', #8197, #14933, #4 ) ;
#8543 = CARTESIAN_POINT ( 'NONE',  ( -21.03221929538690205, 295.1198905765656377, 18.47759065022572500 ) ) ;
#8544 = CARTESIAN_POINT ( 'NONE',  ( 20.74841189052421697, 600.7448905601785327, 7.500000000000000000 ) ) ;
#8545 = CARTESIAN_POINT ( 'NONE',  ( -14.48388495494898542, 257.9323905683720000, 9.489475012073731008 ) ) ;
#8546 = CARTESIAN_POINT ( 'NONE',  ( -8.685887942688735208, 466.9948905765656377, -2.449293598294705724E-15 ) ) ;
#8547 = ADVANCED_FACE ( 'NONE', ( #18449 ), #17051, .F. ) ;
#8548 = CARTESIAN_POINT ( 'NONE',  ( -38.17536295476246266, 413.8073905683719431, -14.20200298773971426 ) ) ;
#8549 = EDGE_CURVE ( 'NONE', #18118, #20734, #3759, .T. ) ;
#8550 = DIRECTION ( 'NONE',  ( 0.000000000000000000, -0.000000000000000000, -1.000000000000000000 ) ) ;
#8551 = CARTESIAN_POINT ( 'NONE',  ( -48.68588794268872988, 537.2448905601785327, 0.000000000000000000 ) ) ;
#8552 = CARTESIAN_POINT ( 'NONE',  ( -8.685887942688902186, 381.9323905601784759, 3.978247347593586447 ) ) ;
#8553 = CARTESIAN_POINT ( 'NONE',  ( -24.70764059509555466, 410.0573905601784759, 19.99999999999998934 ) ) ;
#8554 = CARTESIAN_POINT ( 'NONE',  ( -19.19641293061498288, 321.9323905683720000, -14.20200298773971603 ) ) ;
#8555 = CARTESIAN_POINT ( 'NONE',  ( -11.93348319268873325, 458.8698905683720000, -2.051577885510841163E-15 ) ) ;
#8556 = ORIENTED_EDGE ( 'NONE', *, *, #2692, .F. ) ;
#8557 = CARTESIAN_POINT ( 'NONE',  ( -10.20829729246299777, 462.8698905601785327, -7.653668647301794969 ) ) ;
#8558 = CARTESIAN_POINT ( 'NONE',  ( -14.48388495494899075, 297.9323905683720000, 9.489475012073732785 ) ) ;
#8559 = CARTESIAN_POINT ( 'NONE',  ( 0.4037800551813712224, -4.058962678540093627, 5.969670414742685338 ) ) ;
#8560 = ORIENTED_EDGE ( 'NONE', *, *, #6348, .F. ) ;
#8561 = CARTESIAN_POINT ( 'NONE',  ( 146.1533239063698772, 600.7448905601785327, -7.500000000000000000 ) ) ;
#8562 = CARTESIAN_POINT ( 'NONE',  ( -8.685887942688719221, 342.5573905601785327, -3.978247347593165895 ) ) ;
#8563 = CARTESIAN_POINT ( 'NONE',  ( -35.09675569278794427, 383.4948905683720000, -15.47720386886985544 ) ) ;
#8564 = DIRECTION ( 'NONE',  ( 0.000000000000000000, 0.000000000000000000, 1.000000000000000000 ) ) ;
#8565 =( NAMED_UNIT ( * ) PLANE_ANGLE_UNIT ( ) SI_UNIT ( $, .RADIAN. ) );
#8566 = CARTESIAN_POINT ( 'NONE',  ( -38.17536295476246266, 422.3073905683720568, -14.20200298773971426 ) ) ;
#8567 = CARTESIAN_POINT ( 'NONE',  ( -22.27502019258946575, 268.4948905683720000, 15.47720386886985189 ) ) ;
#8568 = CARTESIAN_POINT ( 'NONE',  ( -28.68588794268871922, 426.3698905683720568, 16.75240474999999307 ) ) ;
#8569 = CARTESIAN_POINT ( 'NONE',  ( -10.20829729246299067, 401.6198905601784759, 7.653668647301790529 ) ) ;
#8570 = CARTESIAN_POINT ( 'NONE',  ( -17.35679799567829917, 358.5573905765655809, -16.95518130045146421 ) ) ;
#8571 = CARTESIAN_POINT ( 'NONE',  ( 60.03793209889851568, 30.52886280891152282, -131.1729372809869005 ) ) ;
#8572 = CYLINDRICAL_SURFACE ( 'NONE', #6117, 19.99999999999999645 ) ;
#8573 = CARTESIAN_POINT ( 'NONE',  ( -35.09675569278794427, 331.9948905683720000, -15.47720386886985544 ) ) ;
#8574 = DIRECTION ( 'NONE',  ( -1.191790137725560488E-16, 1.000000000000000000, -0.000000000000000000 ) ) ;
#8575 = CARTESIAN_POINT ( 'NONE',  ( -19.19641293061499354, 478.8073905683720568, 14.20200298773971426 ) ) ;
#8576 = CARTESIAN_POINT ( 'NONE',  ( -48.68588794268880804, 432.3073905765656377, 3.978247347592954952 ) ) ;
#8577 = CYLINDRICAL_SURFACE ( 'NONE', #5859, 4.000000000000000000 ) ;
#8578 = CARTESIAN_POINT ( 'NONE',  ( -8.685887942688449215, 302.5573905601784759, -3.978247347592526850 ) ) ;
#8579 = CARTESIAN_POINT ( 'NONE',  ( -38.17536295476244845, 386.9323905683721136, 14.20200298773971781 ) ) ;
#8580 = DIRECTION ( 'NONE',  ( 1.191790137725560488E-16, -1.000000000000000000, -0.000000000000000000 ) ) ;
#8581 = CARTESIAN_POINT ( 'NONE',  ( -24.70764059509558308, 524.4323905601785327, -19.99999999999999289 ) ) ;
#8582 = CARTESIAN_POINT ( 'NONE',  ( -32.01814843081344719, 366.0573905683720000, 16.75240474999999307 ) ) ;
#8583 = AXIS2_PLACEMENT_3D ( 'NONE', #3104, #4933, #1703 ) ;
#8584 = ORIENTED_EDGE ( 'NONE', *, *, #15971, .F. ) ;
#8585 = CARTESIAN_POINT ( 'NONE',  ( -38.17536295476247687, 532.3073905683719431, -14.20200298773971426 ) ) ;
#8586 = ORIENTED_EDGE ( 'NONE', *, *, #1622, .F. ) ;
#8587 = CARTESIAN_POINT ( 'NONE',  ( -42.88789093042845479, 514.8073905683720568, 9.489475012073736337 ) ) ;
#8588 = VERTEX_POINT ( 'NONE', #20289 ) ;
#8589 = CARTESIAN_POINT ( 'NONE',  ( -48.68588794268880804, 427.5573905601784190, 3.978247347592954952 ) ) ;
#8590 = CARTESIAN_POINT ( 'NONE',  ( -13.20868407381887621, 489.4948905683720568, -6.410867750099233042 ) ) ;
#8591 = EDGE_LOOP ( 'NONE', ( #8375, #20765, #4503, #7436 ) ) ;
#8592 = CARTESIAN_POINT ( 'NONE',  ( -35.09675569278795848, 481.9948905683720000, -15.47720386886985544 ) ) ;
#8593 = CARTESIAN_POINT ( 'NONE',  ( -42.82802356641967378, 488.4948905601784759, 14.14213562373094923 ) ) ;
#8594 = CARTESIAN_POINT ( 'NONE',  ( -32.66413529028188378, 419.8073905765655809, -19.99999999999999289 ) ) ;
#8595 = CARTESIAN_POINT ( 'NONE',  ( -162.2727221670389781, 30.52886280891152282, 20.57735571454641033 ) ) ;
#8596 = FACE_OUTER_BOUND ( 'NONE', #2227, .T. ) ;
#8597 = CARTESIAN_POINT ( 'NONE',  ( -24.70764059509556887, 439.1823905765655809, -19.99999999999999289 ) ) ;
#8598 = DIRECTION ( 'NONE',  ( -0.000000000000000000, -0.000000000000000000, -1.000000000000000000 ) ) ;
#8599 = VECTOR ( 'NONE', #5459, 1000.000000000000000 ) ;
#8600 = CARTESIAN_POINT ( 'NONE',  ( -32.66413529028188378, 494.1823905765655240, 19.99999999999999289 ) ) ;
#8601 = CARTESIAN_POINT ( 'NONE',  ( -40.53162694259543031, 296.6198905683720000, 11.84573899990672885 ) ) ;
#8602 = FACE_OUTER_BOUND ( 'NONE', #7410, .T. ) ;
#8603 = CARTESIAN_POINT ( 'NONE',  ( -45.43829269268871940, 445.3698905683720000, 0.000000000000000000 ) ) ;
#8604 = CARTESIAN_POINT ( 'NONE',  ( -22.30770786884144741, 45.31613216062291372, -122.9933582338429687 ) ) ;
#8605 = CARTESIAN_POINT ( 'NONE',  ( -45.43829269268869808, 295.0573905683720000, -3.332260488124726194 ) ) ;
#8606 = ORIENTED_EDGE ( 'NONE', *, *, #21219, .T. ) ;
#8607 = CARTESIAN_POINT ( 'NONE',  ( -17.35679799567831694, 533.8073905601784190, -16.95518130045146421 ) ) ;
#8608 = CARTESIAN_POINT ( 'NONE',  ( -28.68588794268873343, 502.8698905683719431, -16.75240474999999307 ) ) ;
#8609 = AXIS2_PLACEMENT_3D ( 'NONE', #14428, #9951, #19588 ) ;
#8610 = EDGE_CURVE ( 'NONE', #5497, #2086, #2126, .T. ) ;
#8611 = ORIENTED_EDGE ( 'NONE', *, *, #1234, .T. ) ;
#8612 = CARTESIAN_POINT ( 'NONE',  ( -22.27502019258949062, 468.4948905683720000, 15.47720386886985189 ) ) ;
#8613 = DIRECTION ( 'NONE',  ( -0.000000000000000000, 1.000000000000000000, -0.000000000000000000 ) ) ;
#8614 = CARTESIAN_POINT ( 'NONE',  ( -45.43829269268869098, 263.5573905683720568, -3.332260488124726194 ) ) ;
#8615 = ORIENTED_EDGE ( 'NONE', *, *, #6301, .F. ) ;
#8616 = SHAPE_REPRESENTATION ( 'hex bolt gradec_iso_ISO 4016 - M8 x 40 x 22-WN', ( #12794 ), #13835 ) ;
#8617 = CARTESIAN_POINT ( 'NONE',  ( -48.68588794268887199, 332.3073905765655240, 3.978247347592742678 ) ) ;
#8618 = AXIS2_PLACEMENT_3D ( 'NONE', #12714, #11291, #14244 ) ;
#8619 = CARTESIAN_POINT ( 'NONE',  ( -19.19641293061496867, 268.8073905683720568, 14.20200298773971426 ) ) ;
#8620 = CARTESIAN_POINT ( 'NONE',  ( -8.685887942688717445, 306.9948905765655809, -2.449293598294705724E-15 ) ) ;
#8621 = PRODUCT_DEFINITION ( 'UNKNOWN', '', #5903, #145 ) ;
#8622 = CARTESIAN_POINT ( 'NONE',  ( -32.01814843081343298, 237.5573905683720568, 16.75240474999999307 ) ) ;
#8623 = CARTESIAN_POINT ( 'NONE',  ( -47.16347859291443712, 307.8698905601784759, 7.653668647301805628 ) ) ;
#8624 = CYLINDRICAL_SURFACE ( 'NONE', #15641, 19.99999999999999645 ) ;
#8625 = CARTESIAN_POINT ( 'NONE',  ( -22.27502019258947641, 260.7448905683720000, -15.47720386886985544 ) ) ;
#8626 = CARTESIAN_POINT ( 'NONE',  ( -45.43829269268871229, 355.3698905683720568, 0.000000000000000000 ) ) ;
#8627 = EDGE_CURVE ( 'NONE', #20033, #9674, #615, .T. ) ;
#8628 = CARTESIAN_POINT ( 'NONE',  ( 2.416697501590669095, 172.9933428177121471, 60.00000000000000000 ) ) ;
#8629 = CARTESIAN_POINT ( 'NONE',  ( -32.01814843081345430, 406.0573905683720000, 16.75240474999999307 ) ) ;
#8630 = CARTESIAN_POINT ( 'NONE',  ( -48.68588794268872277, 507.2448905601785327, 0.000000000000000000 ) ) ;
#8631 = VECTOR ( 'NONE', #13456, 1000.000000000000000 ) ;
#8632 = CARTESIAN_POINT ( 'NONE',  ( -11.73070664223725501, 403.1823905601785327, -11.32908994701042715 ) ) ;
#8633 = ADVANCED_FACE ( 'NONE', ( #10641, #2336 ), #13802, .F. ) ;
#8634 = EDGE_LOOP ( 'NONE', ( #19790, #9893, #15765, #6610 ) ) ;
#8635 = CARTESIAN_POINT ( 'NONE',  ( 0.05613245601076728708, 1.278525034532176585, -6.499999999999999112 ) ) ;
#8636 = ORIENTED_EDGE ( 'NONE', *, *, #3786, .F. ) ;
#8637 = EDGE_LOOP ( 'NONE', ( #11329, #5847, #793, #14062 ) ) ;
#8638 = CARTESIAN_POINT ( 'NONE',  ( -14.48388495494901740, 519.4323905683720568, 9.489475012073732785 ) ) ;
#8639 = CARTESIAN_POINT ( 'NONE',  ( -8.685887942688712116, 281.9323905601784759, 3.978247347593161010 ) ) ;
#8640 = CARTESIAN_POINT ( 'NONE',  ( -48.68588794268870146, 321.9948905765655809, 0.000000000000000000 ) ) ;
#8641 = CARTESIAN_POINT ( 'NONE',  ( -42.88789093042842637, 316.3073905683721136, 9.489475012073734561 ) ) ;
#8642 = VERTEX_POINT ( 'NONE', #1043 ) ;
#8643 = CARTESIAN_POINT ( 'NONE',  ( -38.17536295476244845, 365.4323905683720000, 14.20200298773971781 ) ) ;
#8644 = CARTESIAN_POINT ( 'NONE',  ( -38.17536295476244845, 375.4323905683720000, 14.20200298773971781 ) ) ;
#8645 = VECTOR ( 'NONE', #15955, 1000.000000000000000 ) ;
#8646 = CARTESIAN_POINT ( 'NONE',  ( -32.66413529028186957, 299.8073905765656377, -19.99999999999999289 ) ) ;
#8647 = VECTOR ( 'NONE', #18264, 1000.000000000000000 ) ;
#8648 = DIRECTION ( 'NONE',  ( -0.000000000000000000, -1.000000000000000000, -0.000000000000000000 ) ) ;
#8649 = CARTESIAN_POINT ( 'NONE',  ( -28.68588794268869790, 256.3698905683720000, 16.75240474999999307 ) ) ;
#8650 = CARTESIAN_POINT ( 'NONE',  ( -42.87301415892787304, 204.0033847496196984, 4.870997244581528385 ) ) ;
#8651 = AXIS2_PLACEMENT_3D ( 'NONE', #15827, #9921, #2620 ) ;
#8652 = CARTESIAN_POINT ( 'NONE',  ( -38.17536295476246266, 423.8073905683720568, -14.20200298773971426 ) ) ;
#8653 = CARTESIAN_POINT ( 'NONE',  ( 35.96497763894178945, 230.5765313837437418, 40.00000000000000000 ) ) ;
#8654 = FACE_OUTER_BOUND ( 'NONE', #10603, .T. ) ;
#8655 = CARTESIAN_POINT ( 'NONE',  ( -48.68588794268871567, 411.9948905765656377, 0.000000000000000000 ) ) ;
#8656 = VECTOR ( 'NONE', #6542, 1000.000000000000000 ) ;
#8657 = DIRECTION ( 'NONE',  ( 1.000000000000000000, 0.000000000000000000, 0.000000000000000000 ) ) ;
#8658 = EDGE_LOOP ( 'NONE', ( #9448, #39, #13231 ) ) ;
#8659 = CARTESIAN_POINT ( 'NONE',  ( -40.53162694259543741, 336.6198905683720000, 11.84573899990672885 ) ) ;
#8660 = CARTESIAN_POINT ( 'NONE',  ( -16.84014894278200103, 467.6198905683720000, 11.84573899990672530 ) ) ;
#8661 = VERTEX_POINT ( 'NONE', #12605 ) ;
#8662 = CARTESIAN_POINT ( 'NONE',  ( -40.01497788969914637, 468.8073905601785327, 16.95518130045146776 ) ) ;
#8663 = CARTESIAN_POINT ( 'NONE',  ( -11.93348319268871194, 288.8698905683720568, -2.051577885510841163E-15 ) ) ;
#8664 = PRESENTATION_LAYER_ASSIGNMENT (  '', '', ( #13177 ) ) ;
#8665 = CARTESIAN_POINT ( 'NONE',  ( -8.685887942688720997, 346.9948905765656377, -2.449293598294705724E-15 ) ) ;
#8666 = ORIENTED_EDGE ( 'NONE', *, *, #5828, .F. ) ;
#8667 = CARTESIAN_POINT ( 'NONE',  ( 51.50493485826542184, 170.1716627696692683, -57.52045949366692668 ) ) ;
#8668 = CARTESIAN_POINT ( 'NONE',  ( -17.35679799567828852, 340.6823905601785896, 16.95518130045146421 ) ) ;
#8669 = CARTESIAN_POINT ( 'NONE',  ( -45.43829269268869808, 294.1823905683720000, 3.332260488124734632 ) ) ;
#8670 = CARTESIAN_POINT ( 'NONE',  ( -16.84014894278199037, 389.1198905683720568, 11.84573899990672530 ) ) ;
#8671 = CARTESIAN_POINT ( 'NONE',  ( -45.64106924314017277, 296.3073905601784190, -11.32908994701042538 ) ) ;
#8672 = DIRECTION ( 'NONE',  ( -1.191790137725560488E-16, 1.000000000000000000, -0.000000000000000000 ) ) ;
#8673 = CARTESIAN_POINT ( 'NONE',  ( -14.48388495494900496, 419.8073905683720000, -9.489475012073736337 ) ) ;
#8674 = CARTESIAN_POINT ( 'NONE',  ( -22.27502019258946220, 258.4948905683720568, 15.47720386886985189 ) ) ;
#8675 = CARTESIAN_POINT ( 'NONE',  ( -11.93348319268872793, 419.1823905683720568, -3.332260488124732856 ) ) ;
#8676 = PRODUCT_CONTEXT ( 'NONE', #20085, 'mechanical' ) ;
#8677 = CARTESIAN_POINT ( 'NONE',  ( -28.68588794268871567, 369.4948905765656377, -19.99999999999999289 ) ) ;
#8678 = DIRECTION ( 'NONE',  ( 0.000000000000000000, 0.000000000000000000, 1.000000000000000000 ) ) ;
#8679 = CARTESIAN_POINT ( 'NONE',  ( -19.19641293061497933, 330.4323905683720568, -14.20200298773971603 ) ) ;
#8680 = CARTESIAN_POINT ( 'NONE',  ( -14.54375231895778597, 488.2448905765656377, -14.14213562373094746 ) ) ;
#8681 = CARTESIAN_POINT ( 'NONE',  ( -25.35362745456399480, 468.1823905683721136, 16.75240474999998952 ) ) ;
#8682 = EDGE_CURVE ( 'NONE', #3367, #19032, #19244, .T. ) ;
#8683 = CARTESIAN_POINT ( 'NONE',  ( -8.685887942688729879, 436.9948905765656377, -2.449293598294705724E-15 ) ) ;
#8684 = DIRECTION ( 'NONE',  ( -0.9283449136418786551, 0.000000000000000000, 0.3717199501173604759 ) ) ;
#8685 = AXIS2_PLACEMENT_3D ( 'NONE', #18488, #2275, #15374 ) ;
#8686 = FACE_OUTER_BOUND ( 'NONE', #3829, .T. ) ;
#8687 = ADVANCED_FACE ( 'NONE', ( #20927 ), #17245, .T. ) ;
#8688 = EDGE_CURVE ( 'NONE', #16558, #13685, #6094, .T. ) ;
#8689 = CARTESIAN_POINT ( 'NONE',  ( -19.19641293061498644, 388.8073905683720568, 14.20200298773971426 ) ) ;
#8690 = DIRECTION ( 'NONE',  ( 0.000000000000000000, -1.000000000000000000, 0.000000000000000000 ) ) ;
#8691 = CARTESIAN_POINT ( 'NONE',  ( -40.01497788969916058, 535.6823905601784190, -16.95518130045146421 ) ) ;
#8692 = CARTESIAN_POINT ( 'NONE',  ( -14.48388495494899608, 347.9323905683720000, 9.489475012073732785 ) ) ;
#8693 = EDGE_LOOP ( 'NONE', ( #14513, #18376, #20125, #19899 ) ) ;
#8694 = CARTESIAN_POINT ( 'NONE',  ( -42.88789093042845479, 522.9323905683720568, -9.489475012073736337 ) ) ;
#8695 = ORIENTED_EDGE ( 'NONE', *, *, #19490, .T. ) ;
#8696 = CARTESIAN_POINT ( 'NONE',  ( -8.685887942688719221, 351.9323905601784759, 3.978247347593161010 ) ) ;
#8697 = CARTESIAN_POINT ( 'NONE',  ( -45.43829269268873361, 513.8698905683720568, 0.000000000000000000 ) ) ;
#8698 = ADVANCED_FACE ( 'NONE', ( #4486 ), #2546, .F. ) ;
#8699 = VERTEX_POINT ( 'NONE', #7821 ) ;
#8700 = LINE ( 'NONE', #15322, #7612 ) ;
#8701 = CARTESIAN_POINT ( 'NONE',  ( -38.17536295476246266, 475.4323905683720568, 14.20200298773971781 ) ) ;
#8702 = ORIENTED_EDGE ( 'NONE', *, *, #14057, .F. ) ;
#8703 = CARTESIAN_POINT ( 'NONE',  ( -16.84014894278200103, 487.6198905683720000, 11.84573899990672530 ) ) ;
#8704 = CARTESIAN_POINT ( 'NONE',  ( -12.69441680977503850, 50.46651949346903621, -46.95261769007076680 ) ) ;
#8705 = CARTESIAN_POINT ( 'NONE',  ( -48.68588794268871567, 431.9948905765656377, 0.000000000000000000 ) ) ;
#8706 = CARTESIAN_POINT ( 'NONE',  ( -32.66413529028188378, 474.1823905765655809, 19.99999999999999289 ) ) ;
#8707 = DIRECTION ( 'NONE',  ( 0.000000000000000000, 1.000000000000000000, -0.000000000000000000 ) ) ;
#8708 = CARTESIAN_POINT ( 'NONE',  ( -14.54375231895778420, 483.4948905601784759, -14.14213562373094746 ) ) ;
#8709 = CARTESIAN_POINT ( 'NONE',  ( 1.631480618821192334E-14, 213.9102039777116602, 24.99999999999999645 ) ) ;
#8710 = LINE ( 'NONE', #14907, #1129 ) ;
#8711 = LINE ( 'NONE', #2130, #9700 ) ;
#8712 = VECTOR ( 'NONE', #1594, 1000.000000000000000 ) ;
#8713 = CARTESIAN_POINT ( 'NONE',  ( -44.16309181155856578, 294.7448905683720568, -6.410867750099231266 ) ) ;
#8714 = LINE ( 'NONE', #9907, #13367 ) ;
#8715 = CARTESIAN_POINT ( 'NONE',  ( -40.53162694259544452, 446.6198905683720568, 11.84573899990672885 ) ) ;
#8716 = CARTESIAN_POINT ( 'NONE',  ( -162.2727221670389781, 30.52886280891152282, 4.999999999999990230 ) ) ;
#8717 = VECTOR ( 'NONE', #4083, 1000.000000000000000 ) ;
#8718 = CARTESIAN_POINT ( 'NONE',  ( -11.93348319268871194, 270.0573905683719431, 3.332260488124728415 ) ) ;
#8719 = EDGE_LOOP ( 'NONE', ( #7707, #18963, #3651, #18993 ) ) ;
#8720 = DIRECTION ( 'NONE',  ( 0.000000000000000000, -1.000000000000000000, 0.000000000000000000 ) ) ;
#8721 = CARTESIAN_POINT ( 'NONE',  ( -14.48388495494901562, 511.3073905683720568, -9.489475012073734561 ) ) ;
#8722 = VERTEX_POINT ( 'NONE', #9128 ) ;
#8723 = CARTESIAN_POINT ( 'NONE',  ( -32.01814843081346140, 457.5573905683720000, 16.75240474999999307 ) ) ;
#8724 = FACE_OUTER_BOUND ( 'NONE', #15376, .T. ) ;
#8725 = CARTESIAN_POINT ( 'NONE',  ( -14.48388495494898898, 269.8073905683720000, -9.489475012073736337 ) ) ;
#8726 = CIRCLE ( 'NONE', #5271, 20.00000000000000355 ) ;
#8727 = ORIENTED_EDGE ( 'NONE', *, *, #4215, .F. ) ;
#8728 = CYLINDRICAL_SURFACE ( 'NONE', #1785, 19.99999999999999645 ) ;
#8729 = CARTESIAN_POINT ( 'NONE',  ( -28.68588794268870501, 272.8698905683720000, -16.75240474999999307 ) ) ;
#8730 = CARTESIAN_POINT ( 'NONE',  ( -10.20829729246299955, 476.3698905765656377, 7.653668647301790529 ) ) ;
#8731 = DIRECTION ( 'NONE',  ( 1.000000000000000000, 0.000000000000000000, 0.000000000000000000 ) ) ;
#8732 = CARTESIAN_POINT ( 'NONE',  ( -13.20868407381884602, 249.7448905683720000, 6.410867750099229490 ) ) ;
#8733 = CARTESIAN_POINT ( 'NONE',  ( -40.01497788969914637, 420.4323905765656377, -16.95518130045146421 ) ) ;
#8734 = CARTESIAN_POINT ( 'NONE',  ( -21.03221929538689494, 230.3698905601784759, 18.47759065022572500 ) ) ;
#8735 = DIRECTION ( 'NONE',  ( 1.000000000000000000, 0.000000000000000000, 0.000000000000000000 ) ) ;
#8736 = CARTESIAN_POINT ( 'NONE',  ( -16.84014894278197616, 250.1198905683720284, -11.84573899990672707 ) ) ;
#8737 = CARTESIAN_POINT ( 'NONE',  ( -19.19641293061498644, 351.9323905683720568, -14.20200298773971603 ) ) ;
#8738 = ADVANCED_FACE ( 'NONE', ( #4588 ), #17572, .F. ) ;
#8739 = CIRCLE ( 'NONE', #15328, 6.500000000000000000 ) ;
#8740 = DIRECTION ( 'NONE',  ( 0.000000000000000000, 1.000000000000000000, -0.000000000000000000 ) ) ;
#8741 = VECTOR ( 'NONE', #3246, 1000.000000000000114 ) ;
#8742 = CARTESIAN_POINT ( 'NONE',  ( -13.20868407381886556, 409.4948905683720000, -6.410867750099233042 ) ) ;
#8743 = EDGE_CURVE ( 'NONE', #21019, #7175, #15750, .T. ) ;
#8744 = CARTESIAN_POINT ( 'NONE',  ( -8.685887942688543362, 337.3073905765656377, -3.978247347592740013 ) ) ;
#8745 =( BOUNDED_CURVE ( )  B_SPLINE_CURVE ( 2, ( #6956, #13677, #7059, #16820, #3715, #10199, #18740, #15516, #10623, #12260, #2010, #13579, #15309, #20268, #15200, #8578, #17239 ),
 .UNSPECIFIED., .F., .T. ) 
 B_SPLINE_CURVE_WITH_KNOTS ( ( 3, 2, 2, 2, 2, 2, 2, 2, 3 ),
 ( 0.7187500000000002220, 0.7207031250000002220, 0.7226562500000002220, 0.7246093750000002220, 0.7265625000000002220, 0.7285156250000003331, 0.7304687500000003331, 0.7324218750000003331, 0.7343750000000003331 ),
 .UNSPECIFIED. ) 
 CURVE ( )  GEOMETRIC_REPRESENTATION_ITEM ( )  RATIONAL_B_SPLINE_CURVE ( ( 0.9999999999999977796, 0.9807852804032326510, 1.000000000000000000, 0.9807852804032304306, 1.000000000000000000, 0.9807852804032304306, 1.000000000000000000, 0.9807852804032304306, 1.000000000000000000, 0.9807852804032304306, 1.000000000000000000, 0.9807852804032304306, 1.000000000000000000, 0.9807852804032304306, 1.000000000000000000, 0.9807852804032270999, 1.000000000000003331 ) ) 
 REPRESENTATION_ITEM ( '' )  );
#8746 = CARTESIAN_POINT ( 'NONE',  ( -21.03221929538691271, 400.3698905601785327, 18.47759065022572500 ) ) ;
#8747 = VERTEX_POINT ( 'NONE', #2764 ) ;
#8748 = CARTESIAN_POINT ( 'NONE',  ( -11.73070664223724791, 347.9323905765655809, -11.32908994701042538 ) ) ;
#8749 = VERTEX_POINT ( 'NONE', #19090 ) ;
#8750 = ORIENTED_EDGE ( 'NONE', *, *, #11205, .F. ) ;
#8751 = CARTESIAN_POINT ( 'NONE',  ( -45.43829269268872650, 525.6823905683719431, 3.332260488124734632 ) ) ;
#8752 = CARTESIAN_POINT ( 'NONE',  ( -45.64106924314017988, 286.3073905601785327, -11.32908994701042715 ) ) ;
#8753 = DIRECTION ( 'NONE',  ( 0.000000000000000000, 0.000000000000000000, -1.000000000000000000 ) ) ;
#8754 = VECTOR ( 'NONE', #9255, 1000.000000000000000 ) ;
#8755 = CARTESIAN_POINT ( 'NONE',  ( -40.53162694259543031, 314.1198905683720568, -11.84573899990672707 ) ) ;
#8756 = EDGE_CURVE ( 'NONE', #11085, #4497, #11710, .T. ) ;
#8757 = CARTESIAN_POINT ( 'NONE',  ( -22.27502019258947286, 336.9948905683720000, 15.47720386886985189 ) ) ;
#8758 = VECTOR ( 'NONE', #13249, 1000.000000000000000 ) ;
#8759 = CARTESIAN_POINT ( 'NONE',  ( -25.35362745456399125, 361.0573905683720000, -16.75240474999999307 ) ) ;
#8760 = CARTESIAN_POINT ( 'NONE',  ( -47.16347859291443712, 291.3698905765655809, -7.653668647301793193 ) ) ;
#8761 = LINE ( 'NONE', #15381, #6188 ) ;
#8762 = CARTESIAN_POINT ( 'NONE',  ( -22.27502019258947641, 270.7448905683720568, -15.47720386886985544 ) ) ;
#8763 = CARTESIAN_POINT ( 'NONE',  ( -42.83955070047271363, 204.4880047785818249, 4.967744786903340426 ) ) ;
#8764 = CARTESIAN_POINT ( 'NONE',  ( -11.93348319268872615, 410.0573905683720000, 3.332260488124728415 ) ) ;
#8765 = EDGE_CURVE ( 'NONE', #16030, #15737, #15961, .T. ) ;
#8766 = PLANE ( 'NONE',  #7847 ) ;
#8767 = CARTESIAN_POINT ( 'NONE',  ( -48.68588794268878672, 502.3073905765656946, 3.978247347593009131 ) ) ;
#8768 = CARTESIAN_POINT ( 'NONE',  ( -228.6858879426887654, 610.7448905601785327, 2.449293598294706434E-14 ) ) ;
#8769 = CARTESIAN_POINT ( 'NONE',  ( -45.43829269268870519, 335.0573905683720568, -3.332260488124726194 ) ) ;
#8770 = CARTESIAN_POINT ( 'NONE',  ( -13.20868407381887266, 459.4948905683720568, -6.410867750099233042 ) ) ;
#8771 = ORIENTED_EDGE ( 'NONE', *, *, #3353, .F. ) ;
#8772 = CARTESIAN_POINT ( 'NONE',  ( -14.54375231895777887, 470.9948905601784759, 14.14213562373094568 ) ) ;
#8773 = CARTESIAN_POINT ( 'NONE',  ( -16.84014894278197616, 277.6198905683720568, 11.84573899990672530 ) ) ;
#8774 = AXIS2_PLACEMENT_3D ( 'NONE', #18511, #11917, #3699 ) ;
#8775 = VERTEX_POINT ( 'NONE', #4273 ) ;
#8776 = ORIENTED_EDGE ( 'NONE', *, *, #7539, .T. ) ;
#8777 = CARTESIAN_POINT ( 'NONE',  ( -28.68588794268872633, 333.8848358243226357, 20.00000000000000000 ) ) ;
#8778 = CARTESIAN_POINT ( 'NONE',  ( -47.16347859291444422, 336.6198905601784759, -7.653668647301793193 ) ) ;
#8779 = CARTESIAN_POINT ( 'NONE',  ( -42.88789093042842637, 304.8073905683720000, 9.489475012073736337 ) ) ;
#8780 = EDGE_CURVE ( 'NONE', #2272, #6352, #1358, .T. ) ;
#8781 = CARTESIAN_POINT ( 'NONE',  ( -32.01814843081344719, 387.5573905683719431, 16.75240474999999307 ) ) ;
#8782 = CARTESIAN_POINT ( 'NONE',  ( -14.54375231895776110, 293.4948905601785327, -14.14213562373094746 ) ) ;
#8783 = CARTESIAN_POINT ( 'NONE',  ( -8.685887942688740537, 516.9948905765655809, -2.449293598294705724E-15 ) ) ;
#8784 = CARTESIAN_POINT ( 'NONE',  ( -44.16309181155857999, 403.2448905683720568, -6.410867750099231266 ) ) ;
#8785 = CARTESIAN_POINT ( 'NONE',  ( -22.27502019258947641, 262.2448905683720000, -15.47720386886985544 ) ) ;
#8786 = CARTESIAN_POINT ( 'NONE',  ( -28.68588794268871922, 416.3698905683720568, 16.75240474999999307 ) ) ;
#8787 = CONTEXT_DEPENDENT_SHAPE_REPRESENTATION ( #13032, #12339 ) ;
#8788 = CARTESIAN_POINT ( 'NONE',  ( -48.68588794268870856, 372.3073905765656377, 3.978247347593168115 ) ) ;
#8789 = FACE_OUTER_BOUND ( 'NONE', #7039, .T. ) ;
#8790 = CARTESIAN_POINT ( 'NONE',  ( -40.53162694259543741, 335.1198905683720568, 11.84573899990672885 ) ) ;
#8791 = CARTESIAN_POINT ( 'NONE',  ( -13.20868407381887444, 480.9948905683720000, -6.410867750099233042 ) ) ;
#8792 = EDGE_CURVE ( 'NONE', #13236, #14199, #14024, .T. ) ;
#8793 = DIRECTION ( 'NONE',  ( -1.000000000000000000, -0.000000000000000000, 0.000000000000000000 ) ) ;
#8794 = CARTESIAN_POINT ( 'NONE',  ( 2.416697501590669095, 217.7548513357008630, -45.00000000000000000 ) ) ;
#8795 = CARTESIAN_POINT ( 'NONE',  ( 60.69669829156632090, 56.85652257517428865, 94.99999999999994316 ) ) ;
#8796 = CARTESIAN_POINT ( 'NONE',  ( -11.93348319268872260, 380.0573905683721136, 3.332260488124728415 ) ) ;
#8797 = DIRECTION ( 'NONE',  ( -0.000000000000000000, -0.000000000000000000, -1.000000000000000000 ) ) ;
#8798 = CARTESIAN_POINT ( 'NONE',  ( -28.68588794268872988, 519.7448905601784190, 19.99999999999999289 ) ) ;
#8799 = CARTESIAN_POINT ( 'NONE',  ( -14.48388495494899786, 339.8073905683720568, -9.489475012073736337 ) ) ;
#8800 = ORIENTED_EDGE ( 'NONE', *, *, #14210, .F. ) ;
#8801 = CARTESIAN_POINT ( 'NONE',  ( -19.19641293061500065, 500.4323905683721136, -14.20200298773971603 ) ) ;
#8802 = ORIENTED_EDGE ( 'NONE', *, *, #8289, .F. ) ;
#8803 = CARTESIAN_POINT ( 'NONE',  ( -21.03221929538690915, 350.3698905601784759, 18.47759065022572500 ) ) ;
#8804 = CARTESIAN_POINT ( 'NONE',  ( 118.4271928232701043, 10.52886280891152104, 40.00000000000000000 ) ) ;
#8805 = PLANE ( 'NONE',  #472 ) ;
#8806 = LINE ( 'NONE', #19082, #16255 ) ;
#8807 = CARTESIAN_POINT ( 'NONE',  ( -22.27502019258949773, 480.7448905683720568, -15.47720386886985544 ) ) ;
#8808 = ORIENTED_EDGE ( 'NONE', *, *, #11864, .F. ) ;
#8809 = CARTESIAN_POINT ( 'NONE',  ( -11.93348319268873681, 489.1823905683720568, -3.332260488124732856 ) ) ;
#8810 = CARTESIAN_POINT ( 'NONE',  ( 0.000000000000000000, 5.629165124598848102, 3.250000000000005329 ) ) ;
#8811 = CARTESIAN_POINT ( 'NONE',  ( -17.35679799567830628, 418.5573905765656377, -16.95518130045146421 ) ) ;
#8812 = CARTESIAN_POINT ( 'NONE',  ( -42.82802356641967378, 473.2448905765655809, 14.14213562373094923 ) ) ;
#8813 = CARTESIAN_POINT ( 'NONE',  ( 60.03793209889851568, 30.52886280891152282, -126.1729372809868863 ) ) ;
#8814 = CARTESIAN_POINT ( 'NONE',  ( -47.16347859291445843, 486.6198905601784759, -7.653668647301793193 ) ) ;
#8815 = CARTESIAN_POINT ( 'NONE',  ( -40.01497788969914637, 483.5573905765655809, 16.95518130045146776 ) ) ;
#8816 = CARTESIAN_POINT ( 'NONE',  ( -42.82802356641964536, 260.7448905765656377, -14.14213562373094746 ) ) ;
#8817 = CARTESIAN_POINT ( 'NONE',  ( -31.26501780185373391, 205.1437886375728965, -5.000000000000001776 ) ) ;
#8818 = EDGE_CURVE ( 'NONE', #1192, #11298, #17676, .T. ) ;
#8819 = CARTESIAN_POINT ( 'NONE',  ( -45.43829269268869808, 275.6823905683720568, 3.332260488124734632 ) ) ;
#8820 = ADVANCED_FACE ( 'NONE', ( #937 ), #17463, .T. ) ;
#8821 = CARTESIAN_POINT ( 'NONE',  ( -21.03221929538690915, 365.1198905765656377, 18.47759065022572500 ) ) ;
#8822 = CARTESIAN_POINT ( 'NONE',  ( -19.19641293061498999, 438.8073905683720000, 14.20200298773971426 ) ) ;
#8823 = PLANE ( 'NONE',  #11289 ) ;
#8824 = CARTESIAN_POINT ( 'NONE',  ( -28.68588794268870146, 267.8698905683720000, 16.75240474999999307 ) ) ;
#8825 = ORIENTED_EDGE ( 'NONE', *, *, #20644, .T. ) ;
#8826 = CARTESIAN_POINT ( 'NONE',  ( -8.685887942688887975, 271.9323905601784759, 3.978247347593586447 ) ) ;
#8827 = CARTESIAN_POINT ( 'NONE',  ( -13.20868407381887444, 480.9948905683720000, -6.410867750099233042 ) ) ;
#8828 = ORIENTED_EDGE ( 'NONE', *, *, #1176, .F. ) ;
#8829 = CARTESIAN_POINT ( 'NONE',  ( -47.16347859291445133, 411.3698905765656377, -7.653668647301793193 ) ) ;
#8830 = CARTESIAN_POINT ( 'NONE',  ( -42.88789093042841927, 264.8073905683721136, 9.489475012073736337 ) ) ;
#8831 = ORIENTED_EDGE ( 'NONE', *, *, #1836, .T. ) ;
#8832 = CARTESIAN_POINT ( 'NONE',  ( 30.42502041961814285, 230.5765313837437418, -40.00000000000000000 ) ) ;
#8833 = CARTESIAN_POINT ( 'NONE',  ( -38.17536295476244845, 273.8073905683720000, -14.20200298773971426 ) ) ;
#8834 = CARTESIAN_POINT ( 'NONE',  ( -36.33955658999052929, 483.8698905765656377, 18.47759065022572500 ) ) ;
#8835 = CYLINDRICAL_SURFACE ( 'NONE', #323, 9.999999999999994671 ) ;
#8836 = CARTESIAN_POINT ( 'NONE',  ( -37.54166915975687857, 223.9102039777117454, -14.57737010498150276 ) ) ;
#8837 = CARTESIAN_POINT ( 'NONE',  ( -16.84014894278197616, 251.6198905683720284, -11.84573899990672707 ) ) ;
#8838 = CARTESIAN_POINT ( 'NONE',  ( -42.88789093042845479, 524.4323905683720568, -9.489475012073736337 ) ) ;
#8839 = CARTESIAN_POINT ( 'NONE',  ( -40.01497788969913216, 373.5573905765656377, 16.95518130045146776 ) ) ;
#8840 = CARTESIAN_POINT ( 'NONE',  ( -32.01814843081343298, 256.0573905683720000, 16.75240474999999307 ) ) ;
#8841 = CARTESIAN_POINT ( 'NONE',  ( -14.48388495494899786, 351.3073905683721136, -9.489475012073736337 ) ) ;
#8842 = CARTESIAN_POINT ( 'NONE',  ( -47.16347859291445843, 506.6198905601784190, -7.653668647301793193 ) ) ;
#8843 = CIRCLE ( 'NONE', #19564, 6.500000000000000888 ) ;
#8844 = CARTESIAN_POINT ( 'NONE',  ( -35.09675569278795138, 401.9948905683720568, -15.47720386886985544 ) ) ;
#8845 = DIRECTION ( 'NONE',  ( 1.000000000000000000, 0.000000000000000000, -0.000000000000000000 ) ) ;
#8846 = CARTESIAN_POINT ( 'NONE',  ( -45.64106924314019409, 398.1823905601784759, 11.32908994701042715 ) ) ;
#8847 = AXIS2_PLACEMENT_3D ( 'NONE', #18079, #6719, #14356 ) ;
#8848 = VERTEX_POINT ( 'NONE', #3185 ) ;
#8849 = CARTESIAN_POINT ( 'NONE',  ( -40.01497788969913927, 350.4323905765655809, -16.95518130045146421 ) ) ;
#8850 = VERTEX_POINT ( 'NONE', #17989 ) ;
#8851 = ORIENTED_EDGE ( 'NONE', *, *, #9944, .F. ) ;
#8852 = CARTESIAN_POINT ( 'NONE',  ( -45.43829269268871940, 505.6823905683720568, 3.332260488124734632 ) ) ;
#8853 = CARTESIAN_POINT ( 'NONE',  ( -47.16347859291443712, 286.6198905601784759, -7.653668647301793193 ) ) ;
#8854 = CARTESIAN_POINT ( 'NONE',  ( -42.82802356641965247, 320.7448905765656377, -14.14213562373094746 ) ) ;
#8855 = ORIENTED_EDGE ( 'NONE', *, *, #5982, .F. ) ;
#8856 = CARTESIAN_POINT ( 'NONE',  ( -16.84014894278198327, 329.1198905683720568, 11.84573899990672530 ) ) ;
#8857 = VERTEX_POINT ( 'NONE', #17882 ) ;
#8858 = CARTESIAN_POINT ( 'NONE',  ( -19.19641293061498288, 347.3073905683720568, 14.20200298773971426 ) ) ;
#8859 = CARTESIAN_POINT ( 'NONE',  ( -40.53162694259543741, 365.1198905683720000, 11.84573899990672885 ) ) ;
#8860 = CIRCLE ( 'NONE', #1281, 15.00000000000000000 ) ;
#8861 = CARTESIAN_POINT ( 'NONE',  ( -40.01497788969913216, 290.4323905765656377, -16.95518130045146421 ) ) ;
#8862 = CARTESIAN_POINT ( 'NONE',  ( -24.70764059509556176, 394.4323905601784190, -19.99999999999999289 ) ) ;
#8863 = CARTESIAN_POINT ( 'NONE',  ( -19.19641293061496867, 250.4323905683720284, -14.20200298773971603 ) ) ;
#8864 = CARTESIAN_POINT ( 'NONE',  ( -48.68588794268860198, 226.9323905601784759, -3.978247347593371508 ) ) ;
#8865 = CARTESIAN_POINT ( 'NONE',  ( -35.09675569278795848, 417.2448905683720568, 15.47720386886985366 ) ) ;
#8866 = AXIS2_PLACEMENT_3D ( 'NONE', #5232, #18738, #7159 ) ;
#8867 = DIRECTION ( 'NONE',  ( 0.000000000000000000, 0.000000000000000000, 1.000000000000000000 ) ) ;
#8868 = CARTESIAN_POINT ( 'NONE',  ( -10.20829729246300310, 506.3698905765656946, 7.653668647301790529 ) ) ;
#8869 =( BOUNDED_CURVE ( )  B_SPLINE_CURVE ( 2, ( #16793, #4199, #12312, #5813, #18902, #1080, #11801, #13437, #12421, #4087, #19016, #10674, #10785, #18398, #9163, #15787, #975 ),
 .UNSPECIFIED., .F., .T. ) 
 B_SPLINE_CURVE_WITH_KNOTS ( ( 3, 2, 2, 2, 2, 2, 2, 2, 3 ),
 ( 0.5468750000000003331, 0.5488281250000003331, 0.5507812500000002220, 0.5527343750000002220, 0.5546875000000002220, 0.5566406250000002220, 0.5585937500000002220, 0.5605468750000001110, 0.5625000000000001110 ),
 .UNSPECIFIED. ) 
 CURVE ( )  GEOMETRIC_REPRESENTATION_ITEM ( )  RATIONAL_B_SPLINE_CURVE ( ( 0.9999999999999966693, 0.9807852804032337612, 1.000000000000000000, 0.9807852804032304306, 1.000000000000000000, 0.9807852804032304306, 1.000000000000000000, 0.9807852804032304306, 1.000000000000000000, 0.9807852804032304306, 1.000000000000000000, 0.9807852804032304306, 1.000000000000000000, 0.9807852804032304306, 1.000000000000000000, 0.9807852804032293204, 1.000000000000001110 ) ) 
 REPRESENTATION_ITEM ( '' )  );
#8870 = LINE ( 'NONE', #674, #11493 ) ;
#8871 = CARTESIAN_POINT ( 'NONE',  ( -40.53162694259543031, 324.1198905683720568, -11.84573899990672707 ) ) ;
#8872 = CARTESIAN_POINT ( 'NONE',  ( -14.48388495494901029, 459.8073905683720000, -9.489475012073736337 ) ) ;
#8873 = ORIENTED_EDGE ( 'NONE', *, *, #14673, .F. ) ;
#8874 = CARTESIAN_POINT ( 'NONE',  ( -8.685887942688733432, 462.2448905601784759, -2.449293598294705724E-15 ) ) ;
#8875 = CARTESIAN_POINT ( 'NONE',  ( -32.01814843081344009, 281.6823905683720568, -16.75240474999999307 ) ) ;
#8876 = CIRCLE ( 'NONE', #973, 20.00000000000000000 ) ;
#8877 = VERTEX_POINT ( 'NONE', #8032 ) ;
#8878 = CARTESIAN_POINT ( 'NONE',  ( -35.09675569278795848, 453.4948905683720568, -15.47720386886985544 ) ) ;
#8879 = ORIENTED_EDGE ( 'NONE', *, *, #13966, .F. ) ;
#8880 = DIRECTION ( 'NONE',  ( 1.000000000000000000, 1.250996701150283068E-16, -0.000000000000000000 ) ) ;
#8881 = CARTESIAN_POINT ( 'NONE',  ( -40.01497788969913927, 345.6823905601784759, -16.95518130045146421 ) ) ;
#8882 = CARTESIAN_POINT ( 'NONE',  ( -25.35362745456398414, 291.0573905683720000, -16.75240474999999307 ) ) ;
#8883 = ADVANCED_FACE ( 'NONE', ( #3295 ), #58, .T. ) ;
#8884 = AXIS2_PLACEMENT_3D ( 'NONE', #16549, #14718, #11448 ) ;
#8885 = CARTESIAN_POINT ( 'NONE',  ( -32.01814843081344719, 383.1823905683720000, -16.75240474999999307 ) ) ;
#8886 = CARTESIAN_POINT ( 'NONE',  ( -10.20829729246297113, 231.6198905601785043, 7.653668647301790529 ) ) ;
#8887 = CARTESIAN_POINT ( 'NONE',  ( -17.35679799567831694, 518.5573905765655809, -16.95518130045146421 ) ) ;
#8888 = CARTESIAN_POINT ( 'NONE',  ( -28.68588794268871922, 406.3698905683720000, 16.75240474999999307 ) ) ;
#8889 = CARTESIAN_POINT ( 'NONE',  ( -11.93348319268870839, 250.0573905683720000, 3.332260488124728415 ) ) ;
#8890 = CARTESIAN_POINT ( 'NONE',  ( -44.16309181155857999, 423.2448905683720568, -6.410867750099231266 ) ) ;
#8891 = ITEM_DEFINED_TRANSFORMATION ( 'NONE', 'NONE', #4175,  #12794 ) ;
#8892 = CARTESIAN_POINT ( 'NONE',  ( -11.73070664223724968, 337.9323905765655809, -11.32908994701042715 ) ) ;
#8893 = FACE_OUTER_BOUND ( 'NONE', #17387, .T. ) ;
#8894 = CARTESIAN_POINT ( 'NONE',  ( -22.27502019258947286, 316.9948905683720568, 15.47720386886985189 ) ) ;
#8895 = CARTESIAN_POINT ( 'NONE',  ( -44.16309181155858710, 484.7448905683720568, -6.410867750099231266 ) ) ;
#8896 = CARTESIAN_POINT ( 'NONE',  ( 0.000000000000000000, 0.000000000000000000, 0.000000000000000000 ) ) ;
#8897 = CARTESIAN_POINT ( 'NONE',  ( -17.35679799567827430, 225.4323905765656093, 16.95518130045146421 ) ) ;
#8898 = EDGE_CURVE ( 'NONE', #2506, #16623, #16389, .T. ) ;
#8899 = CARTESIAN_POINT ( 'NONE',  ( -40.53162694259543741, 386.6198905683720568, 11.84573899990672885 ) ) ;
#8900 = CARTESIAN_POINT ( 'NONE',  ( -26.35054759312642503, 46.04092669597897469, -122.1915506529835653 ) ) ;
#8901 = CARTESIAN_POINT ( 'NONE',  ( -42.82802356641968089, 518.4948905601785327, 14.14213562373094923 ) ) ;
#8902 = CARTESIAN_POINT ( 'NONE',  ( -25.35362745456398770, 341.0573905683720000, -16.75240474999999307 ) ) ;
#8903 = VERTEX_POINT ( 'NONE', #13134 ) ;
#8904 = CARTESIAN_POINT ( 'NONE',  ( -40.53162694259545162, 502.6198905683720568, -11.84573899990672707 ) ) ;
#8905 = ORIENTED_EDGE ( 'NONE', *, *, #6720, .F. ) ;
#8906 = CARTESIAN_POINT ( 'NONE',  ( -41.29049502611874090, 223.9102039777116033, -11.05440166866015694 ) ) ;
#8907 = CARTESIAN_POINT ( 'NONE',  ( -28.68588794268875120, 610.7448905601785327, 0.000000000000000000 ) ) ;
#8908 = EDGE_CURVE ( 'NONE', #16932, #1213, #5154, .T. ) ;
#8909 = CARTESIAN_POINT ( 'NONE',  ( 292.4526463419396691, 308.2087638784415162, -20.00000000000000355 ) ) ;
#8910 = CARTESIAN_POINT ( 'NONE',  ( -40.01497788969916058, 520.4323905765656946, -16.95518130045146421 ) ) ;
#8911 = CARTESIAN_POINT ( 'NONE',  ( -11.93348319268873325, 458.5573905683720568, 3.332260488124728415 ) ) ;
#8912 = ORIENTED_EDGE ( 'NONE', *, *, #17514, .F. ) ;
#8913 = CARTESIAN_POINT ( 'NONE',  ( -42.88789093042844769, 494.8073905683720000, 9.489475012073734561 ) ) ;
#8914 = CARTESIAN_POINT ( 'NONE',  ( -8.685887942688708563, 252.2448905601784475, -2.449293598294705724E-15 ) ) ;
#8915 = CARTESIAN_POINT ( 'NONE',  ( -48.68588794268871567, 412.3073905765655809, 3.978247347593168115 ) ) ;
#8916 = CARTESIAN_POINT ( 'NONE',  ( -162.2727221670389781, 30.52886280891152282, 0.000000000000000000 ) ) ;
#8917 = CARTESIAN_POINT ( 'NONE',  ( 8.938426032941704028E-16, 585.7448905601785327, 7.500000000000000000 ) ) ;
#8918 = FACE_OUTER_BOUND ( 'NONE', #11911, .T. ) ;
#8919 = DIRECTION ( 'NONE',  ( 0.000000000000000000, 1.000000000000000000, -0.000000000000000000 ) ) ;
#8920 = CARTESIAN_POINT ( 'NONE',  ( 10.41669750159067220, 172.9933428177121471, -60.00000000000000000 ) ) ;
#8921 = CARTESIAN_POINT ( 'NONE',  ( -21.03221929538693047, 434.1198905601784759, -18.47759065022572855 ) ) ;
#8922 = DIRECTION ( 'NONE',  ( -1.232945044042657126E-32, 9.855701800883825964E-17, 1.000000000000000000 ) ) ;
#8923 = CARTESIAN_POINT ( 'NONE',  ( -11.93348319268871194, 280.0573905683720568, 3.332260488124728415 ) ) ;
#8924 = CIRCLE ( 'NONE', #3756, 6.500000000000000000 ) ;
#8925 = CARTESIAN_POINT ( 'NONE',  ( -45.64106924314017277, 258.1823905601784759, 11.32908994701042715 ) ) ;
#8926 = CARTESIAN_POINT ( 'NONE',  ( -28.68588794268872277, 437.8698905683720568, 16.75240474999999307 ) ) ;
#8927 = CARTESIAN_POINT ( 'NONE',  ( 158.8141120573112630, 400.5398297725602674, 9.999999999999994671 ) ) ;
#8928 = CARTESIAN_POINT ( 'NONE',  ( -14.48388495494898898, 271.3073905683720568, -9.489475012073736337 ) ) ;
#8929 = EDGE_LOOP ( 'NONE', ( #8482, #15368, #3698, #4039, #20463, #989 ) ) ;
#8930 = CARTESIAN_POINT ( 'NONE',  ( -48.68588794268861619, 481.6823905765655809, -3.978247347593425243 ) ) ;
#8931 = ORIENTED_EDGE ( 'NONE', *, *, #3638, .T. ) ;
#8932 = CARTESIAN_POINT ( 'NONE',  ( -14.48388495494901029, 489.4323905683720000, 9.489475012073731008 ) ) ;
#8933 = ORIENTED_EDGE ( 'NONE', *, *, #16446, .F. ) ;
#8934 = CARTESIAN_POINT ( 'NONE',  ( -28.68588794268874054, 573.2448905601785327, 0.000000000000000000 ) ) ;
#8935 = CARTESIAN_POINT ( 'NONE',  ( -19.19641293061496867, 237.3073905683720284, 14.20200298773971426 ) ) ;
#8936 = ADVANCED_FACE ( 'NONE', ( #4906 ), #14663, .T. ) ;
#8937 = ORIENTED_EDGE ( 'NONE', *, *, #20917, .F. ) ;
#8938 = DIRECTION ( 'NONE',  ( -1.000000000000000000, 0.000000000000000000, 0.000000000000000000 ) ) ;
#8939 = VECTOR ( 'NONE', #6177, 1000.000000000000000 ) ;
#8940 = CARTESIAN_POINT ( 'NONE',  ( -48.68588794268872277, 481.9948905765656377, 0.000000000000000000 ) ) ;
#8941 = CARTESIAN_POINT ( 'NONE',  ( -48.68588794268870856, 387.2448905601784759, 0.000000000000000000 ) ) ;
#8942 = CARTESIAN_POINT ( 'NONE',  ( -19.52302674270934801, 223.9102039777117454, -17.65796940415495087 ) ) ;
#8943 = CARTESIAN_POINT ( 'NONE',  ( 115.7989814974898195, 160.1716627696691830, 20.00000000000000355 ) ) ;
#8944 = CARTESIAN_POINT ( 'NONE',  ( -11.93348319268874036, 520.3698905683720568, -2.051577885510841163E-15 ) ) ;
#8945 = CARTESIAN_POINT ( 'NONE',  ( -8.685887942688724550, 376.9948905765655809, -2.449293598294705724E-15 ) ) ;
#8946 = CARTESIAN_POINT ( 'NONE',  ( -45.43829269268869098, 243.5573905683720000, -3.332260488124726194 ) ) ;
#8947 = CARTESIAN_POINT ( 'NONE',  ( -13.20868407381885845, 340.9948905683720000, -6.410867750099233042 ) ) ;
#8948 = EDGE_CURVE ( 'NONE', #16161, #258, #15629, .T. ) ;
#8949 = CARTESIAN_POINT ( 'NONE',  ( -28.68588794268870856, 319.7448905601785327, 19.99999999999999289 ) ) ;
#8950 = EDGE_CURVE ( 'NONE', #16730, #8313, #12046, .T. ) ;
#8951 = VECTOR ( 'NONE', #17207, 1000.000000000000000 ) ;
#8952 = EDGE_CURVE ( 'NONE', #19571, #6011, #4107, .T. ) ;
#8953 = CARTESIAN_POINT ( 'NONE',  ( -44.16309181155857999, 403.2448905683720568, -6.410867750099231266 ) ) ;
#8954 = CARTESIAN_POINT ( 'NONE',  ( -42.88789093042845479, 534.4323905683719431, -9.489475012073734561 ) ) ;
#8955 = CARTESIAN_POINT ( 'NONE',  ( -36.33955658999051508, 379.1198905601784759, 18.47759065022572500 ) ) ;
#8956 = EDGE_LOOP ( 'NONE', ( #8985, #14170, #18827, #12435 ) ) ;
#8957 = DIRECTION ( 'NONE',  ( -1.000000000000000000, -0.000000000000000000, -0.000000000000000000 ) ) ;
#8958 = EDGE_LOOP ( 'NONE', ( #15207, #15586 ) ) ;
#8959 = ORIENTED_EDGE ( 'NONE', *, *, #12797, .F. ) ;
#8960 = CARTESIAN_POINT ( 'NONE',  ( -42.88789093042845479, 506.3073905683720568, 9.489475012073736337 ) ) ;
#8961 = CYLINDRICAL_SURFACE ( 'NONE', #17327, 4.000000000000001776 ) ;
#8962 = ORIENTED_EDGE ( 'NONE', *, *, #662, .T. ) ;
#8963 = EDGE_CURVE ( 'NONE', #4099, #4363, #13354, .T. ) ;
#8964 = CARTESIAN_POINT ( 'NONE',  ( -13.20868407381885490, 310.9948905683720568, -6.410867750099233042 ) ) ;
#8965 = ORIENTED_EDGE ( 'NONE', *, *, #21038, .F. ) ;
#8966 = CARTESIAN_POINT ( 'NONE',  ( -11.93348319268872260, 348.5573905683720000, 3.332260488124728415 ) ) ;
#8967 = CARTESIAN_POINT ( 'NONE',  ( -38.17536295476244845, 345.4323905683719431, 14.20200298773971781 ) ) ;
#8968 = CARTESIAN_POINT ( 'NONE',  ( -42.82802356641965247, 280.7448905765655809, -14.14213562373094746 ) ) ;
#8969 = CARTESIAN_POINT ( 'NONE',  ( -18.68588794268873698, 323.8848358243226357, 40.00000000000000000 ) ) ;
#8970 = CARTESIAN_POINT ( 'NONE',  ( -40.53162694259542320, 252.6198905683720284, -11.84573899990672707 ) ) ;
#8971 = CARTESIAN_POINT ( 'NONE',  ( 147.4234352242185935, 620.7448905601785327, 1.893624729818134345 ) ) ;
#8972 = CARTESIAN_POINT ( 'NONE',  ( -32.01814843081345430, 397.5573905683721136, 16.75240474999999307 ) ) ;
#8973 = CARTESIAN_POINT ( 'NONE',  ( 0.000000000000000000, 7.960204194457796463E-16, -6.500000000000000888 ) ) ;
#8974 = CARTESIAN_POINT ( 'NONE',  ( -10.20829729246298356, 352.8698905601784759, -7.653668647301794969 ) ) ;
#8975 = UNCERTAINTY_MEASURE_WITH_UNIT (LENGTH_MEASURE( 1.000000000000000082E-05 ), #15936, 'distance_accuracy_value', 'NONE');
#8976 = CARTESIAN_POINT ( 'NONE',  ( 151.4788465195079823, 610.7448905601785327, -8.917803138848077182 ) ) ;
#8977 = CARTESIAN_POINT ( 'NONE',  ( -35.09675569278794427, 317.2448905683720000, 15.47720386886985366 ) ) ;
#8978 = CARTESIAN_POINT ( 'NONE',  ( -45.43829269268872650, 453.8698905683720000, 0.000000000000000000 ) ) ;
#8979 = ORIENTED_EDGE ( 'NONE', *, *, #2184, .T. ) ;
#8980 = CARTESIAN_POINT ( 'NONE',  ( -32.66413529028189089, 459.4323905601784759, 19.99999999999999289 ) ) ;
#8981 = CARTESIAN_POINT ( 'NONE',  ( -44.16309181155856578, 283.2448905683720568, -6.410867750099231266 ) ) ;
#8982 = VERTEX_POINT ( 'NONE', #10509 ) ;
#8983 = AXIS2_PLACEMENT_3D ( 'NONE', #14984, #11723, #18315 ) ;
#8984 = LINE ( 'NONE', #17323, #20843 ) ;
#8985 = ORIENTED_EDGE ( 'NONE', *, *, #11593, .F. ) ;
#8986 = ORIENTED_EDGE ( 'NONE', *, *, #2295, .F. ) ;
#8987 = DIRECTION ( 'NONE',  ( 1.000000000000000000, 0.000000000000000000, 0.000000000000000000 ) ) ;
#8988 = CARTESIAN_POINT ( 'NONE',  ( -32.01814843081344009, 301.6823905683720568, -16.75240474999999307 ) ) ;
#8989 = CARTESIAN_POINT ( 'NONE',  ( -25.35362745456399125, 362.5573905683720568, -16.75240474999999307 ) ) ;
#8990 = AXIS2_PLACEMENT_3D ( 'NONE', #9576, #9891, #21261 ) ;
#8991 = CARTESIAN_POINT ( 'NONE',  ( -8.685887942688546914, 372.5573905601784190, -3.978247347592740013 ) ) ;
#8992 = CARTESIAN_POINT ( 'NONE',  ( -28.68588794268872988, 514.4948905765655809, 19.99999999999999289 ) ) ;
#8993 = CARTESIAN_POINT ( 'NONE',  ( -19.19641293061498644, 397.3073905683720000, 14.20200298773971426 ) ) ;
#8994 = CARTESIAN_POINT ( 'NONE',  ( -38.17536295476244135, 233.8073905683720284, -14.20200298773971426 ) ) ;
#8995 = CARTESIAN_POINT ( 'NONE',  ( -42.88789093042844058, 404.8073905683721136, 9.489475012073734561 ) ) ;
#8996 = ITEM_DEFINED_TRANSFORMATION ( 'NONE', 'NONE', #19350,  #12794 ) ;
#8997 = CARTESIAN_POINT ( 'NONE',  ( -48.68588794268870856, 352.3073905765656377, 3.978247347593168115 ) ) ;
#8998 = CARTESIAN_POINT ( 'NONE',  ( 65.85920792673738333, 160.1716627696692683, -20.00000000000000355 ) ) ;
#8999 = CARTESIAN_POINT ( 'NONE',  ( -14.48388495494899075, 297.9323905683720000, 9.489475012073731008 ) ) ;
#9000 = CARTESIAN_POINT ( 'NONE',  ( -16.84014894278200103, 461.6198905683720568, -11.84573899990672707 ) ) ;
#9001 = CARTESIAN_POINT ( 'NONE',  ( -8.685887942688886199, 461.9323905601784190, 3.978247347593533600 ) ) ;
#9002 = CARTESIAN_POINT ( 'NONE',  ( 118.4271928232701043, 10.52886280891152104, -40.00000000000000000 ) ) ;
#9003 = DIRECTION ( 'NONE',  ( 1.374938938973709817E-16, -1.000000000000000000, 0.000000000000000000 ) ) ;
#9004 = EDGE_CURVE ( 'NONE', #17095, #19877, #10381, .T. ) ;
#9005=STYLED_ITEM('',(#21442),#12085);
#9006 = CARTESIAN_POINT ( 'NONE',  ( -22.27502019258947641, 368.4948905683720568, 15.47720386886985189 ) ) ;
#9007 = DIRECTION ( 'NONE',  ( -1.191790137725560488E-16, 1.000000000000000000, -0.000000000000000000 ) ) ;
#9008 = CARTESIAN_POINT ( 'NONE',  ( -24.70764059509556887, 520.0573905601784190, 19.99999999999998934 ) ) ;
#9009 = CARTESIAN_POINT ( 'NONE',  ( -38.17536295476244845, 335.4323905683720000, 14.20200298773971781 ) ) ;
#9010 = ORIENTED_EDGE ( 'NONE', *, *, #12854, .F. ) ;
#9011 = CARTESIAN_POINT ( 'NONE',  ( -11.93348319268873858, 509.1823905683719431, -3.332260488124732856 ) ) ;
#9012 = ORIENTED_EDGE ( 'NONE', *, *, #18289, .T. ) ;
#9013 = CARTESIAN_POINT ( 'NONE',  ( -40.84173908167358036, 223.9102039777116033, -11.54621117671109864 ) ) ;
#9014 = CARTESIAN_POINT ( 'NONE',  ( -11.73070664223724080, 316.0573905765655809, 11.32908994701042005 ) ) ;
#9015 = B_SPLINE_CURVE_WITH_KNOTS ( 'NONE', 3,
 ( #19976, #8392, #13060, #15124, #306, #5155, #18348, #4826, #19646, #13170 ),
 .UNSPECIFIED., .F., .F.,
 ( 4, 2, 2, 2, 4 ),
 ( 0.5000000000000000000, 0.5416256048145712265, 0.5832512096291423420, 0.6248768144437135685, 0.6665024192582847951 ),
 .UNSPECIFIED. ) ;
#9016 = CARTESIAN_POINT ( 'NONE',  ( 5.674999999999999822, -7.505553499465148271, 0.000000000000000000 ) ) ;
#9017 = CARTESIAN_POINT ( 'NONE',  ( -17.35679799567831694, 518.5573905765655809, -16.95518130045146421 ) ) ;
#9018 = CARTESIAN_POINT ( 'NONE',  ( -40.53162694259545162, 455.1198905683720568, 11.84573899990672885 ) ) ;
#9019 = ORIENTED_EDGE ( 'NONE', *, *, #11734, .F. ) ;
#9020 = CARTESIAN_POINT ( 'NONE',  ( -28.68588794268872633, 476.3698905683720568, 16.75240474999999307 ) ) ;
#9021 = EDGE_CURVE ( 'NONE', #15047, #2858, #5540, .T. ) ;
#9022 = CARTESIAN_POINT ( 'NONE',  ( -45.64106924314019409, 412.9323905765655809, 11.32908994701042715 ) ) ;
#9023 = DIRECTION ( 'NONE',  ( -0.000000000000000000, -0.000000000000000000, 1.000000000000000000 ) ) ;
#9024 = CARTESIAN_POINT ( 'NONE',  ( -24.70764059509554045, 300.0573905601784759, 19.99999999999998934 ) ) ;
#9025 = DIRECTION ( 'NONE',  ( -1.000000000000000000, 0.000000000000000000, 0.000000000000000000 ) ) ;
#9026 = DIRECTION ( 'NONE',  ( -1.000000000000000000, 0.000000000000000000, 0.000000000000000000 ) ) ;
#9027 = CARTESIAN_POINT ( 'NONE',  ( -40.01497788969912506, 260.4323905765656377, -16.95518130045146421 ) ) ;
#9028 = DIRECTION ( 'NONE',  ( 0.000000000000000000, 1.000000000000000000, -0.000000000000000000 ) ) ;
#9029 = CARTESIAN_POINT ( 'NONE',  ( -11.93348319268871371, 280.6823905683720000, -3.332260488124732856 ) ) ;
#9030 = EDGE_CURVE ( 'NONE', #3989, #19427, #489, .T. ) ;
#9031 = CARTESIAN_POINT ( 'NONE',  ( -40.01497788969911795, 258.8073905601784759, 16.95518130045146776 ) ) ;
#9032 = CARTESIAN_POINT ( 'NONE',  ( -28.68588794268872277, 333.8848358243226357, -20.00000000000000000 ) ) ;
#9033 = ADVANCED_FACE ( 'NONE', ( #5120 ), #10192, .F. ) ;
#9034 = CARTESIAN_POINT ( 'NONE',  ( -14.48388495494900496, 439.4323905683720000, 9.489475012073732785 ) ) ;
#9035 = LINE ( 'NONE', #17377, #17502 ) ;
#9036 = CARTESIAN_POINT ( 'NONE',  ( -38.17536295476243424, 266.9323905683720000, 14.20200298773971781 ) ) ;
#9037 = ORIENTED_EDGE ( 'NONE', *, *, #12205, .F. ) ;
#9038 = CARTESIAN_POINT ( 'NONE',  ( -10.20829729246299955, 477.6198905765656377, -7.653668647301794969 ) ) ;
#9039 = CIRCLE ( 'NONE', #7980, 6.500000000000000888 ) ;
#9040 = VERTEX_POINT ( 'NONE', #16814 ) ;
#9041 = CARTESIAN_POINT ( 'NONE',  ( -28.68588794268872633, 487.8698905683720568, 16.75240474999999307 ) ) ;
#9042 = EDGE_LOOP ( 'NONE', ( #6058, #16133, #12293, #20673 ) ) ;
#9043 = CARTESIAN_POINT ( 'NONE',  ( 18.55315245287936321, 213.9102039777116602, 25.00000000000000000 ) ) ;
#9044 = CARTESIAN_POINT ( 'NONE',  ( -14.48388495494898365, 247.9323905683720284, 9.489475012073732785 ) ) ;
#9045 = ORIENTED_EDGE ( 'NONE', *, *, #4427, .F. ) ;
#9046 = LINE ( 'NONE', #12301, #1767 ) ;
#9047 = CARTESIAN_POINT ( 'NONE',  ( -28.68588794268872988, 469.4948905765656377, -19.99999999999999289 ) ) ;
#9048 = PRODUCT_DEFINITION_SHAPE ( 'NONE', 'NONE',  #21394 ) ;
#9049 = DIRECTION ( 'NONE',  ( -1.191790137725560488E-16, 1.000000000000000000, -0.000000000000000000 ) ) ;
#9050 = CARTESIAN_POINT ( 'NONE',  ( -33.72690641870477180, 223.9102039777116886, -17.05470716272690979 ) ) ;
#9051 = DIRECTION ( 'NONE',  ( -1.000000000000000000, -1.191790137725560488E-16, 0.000000000000000000 ) ) ;
#9052 = CARTESIAN_POINT ( 'NONE',  ( -28.68588794268873343, 512.8698905683719431, -16.75240474999999307 ) ) ;
#9053 = CARTESIAN_POINT ( 'NONE',  ( -42.82802356641965957, 373.2448905765656377, 14.14213562373094923 ) ) ;
#9054 = SHAPE_REPRESENTATION_RELATIONSHIP ( 'NONE' , 'NONE' ,  #4076, #5838 ) ;
#9055 = CARTESIAN_POINT ( 'NONE',  ( -25.35362745456397704, 241.0573905683720284, -16.75240474999999307 ) ) ;
#9056 = VECTOR ( 'NONE', #1214, 1000.000000000000000 ) ;
#9057 = CARTESIAN_POINT ( 'NONE',  ( -16.84014894278198327, 329.1198905683720568, 11.84573899990672530 ) ) ;
#9058 = CARTESIAN_POINT ( 'NONE',  ( -45.64106924314017277, 318.1823905601784759, 11.32908994701042538 ) ) ;
#9059 = CARTESIAN_POINT ( 'NONE',  ( -21.03221929538690205, 275.1198905765655809, 18.47759065022572500 ) ) ;
#9060 = CARTESIAN_POINT ( 'NONE',  ( -45.43829269268871229, 373.8698905683720000, 0.000000000000000000 ) ) ;
#9061 = PLANE ( 'NONE',  #13972 ) ;
#9062 = VECTOR ( 'NONE', #4379, 1000.000000000000000 ) ;
#9063 = CARTESIAN_POINT ( 'NONE',  ( -8.685887942688726326, 392.2448905601784759, -2.449293598294705724E-15 ) ) ;
#9064 = ORIENTED_EDGE ( 'NONE', *, *, #12639, .T. ) ;
#9065 = CARTESIAN_POINT ( 'NONE',  ( -36.33955658999050797, 350.1198905765656377, -18.47759065022572855 ) ) ;
#9066 = ORIENTED_EDGE ( 'NONE', *, *, #19266, .F. ) ;
#9067 = VERTEX_POINT ( 'NONE', #12146 ) ;
#9068 = CARTESIAN_POINT ( 'NONE',  ( -38.17536295476246977, 516.9323905683720568, 14.20200298773971781 ) ) ;
#9069 = LINE ( 'NONE', #17512, #14572 ) ;
#9070 = ORIENTED_EDGE ( 'NONE', *, *, #17868, .F. ) ;
#9071 = CARTESIAN_POINT ( 'NONE',  ( -16.84014894278197971, 299.1198905683720000, 11.84573899990672530 ) ) ;
#9072 = ORIENTED_EDGE ( 'NONE', *, *, #17082, .T. ) ;
#9073 = CARTESIAN_POINT ( 'NONE',  ( -25.35362745456397704, 336.6823905683720568, 16.75240474999998952 ) ) ;
#9074 = ADVANCED_FACE ( 'NONE', ( #3919 ), #20051, .T. ) ;
#9075 = CARTESIAN_POINT ( 'NONE',  ( -11.93348319268872260, 338.5573905683720568, 3.332260488124728859 ) ) ;
#9076 = CARTESIAN_POINT ( 'NONE',  ( -10.20829729246297646, 277.6198905765655809, -7.653668647301794969 ) ) ;
#9077 = CARTESIAN_POINT ( 'NONE',  ( -42.82802356641966668, 395.9948905601784759, -14.14213562373094746 ) ) ;
#9078 = CARTESIAN_POINT ( 'NONE',  ( -13.20868407381884779, 239.4948905683720284, -6.410867750099233042 ) ) ;
#9079 = DIRECTION ( 'NONE',  ( -0.000000000000000000, -0.000000000000000000, 1.000000000000000000 ) ) ;
#9080 = VECTOR ( 'NONE', #21090, 1000.000000000000114 ) ;
#9081 = CARTESIAN_POINT ( 'NONE',  ( -45.43829269268871940, 395.3698905683720000, 0.000000000000000000 ) ) ;
#9082 = DIRECTION ( 'NONE',  ( 0.000000000000000000, 1.000000000000000000, 0.000000000000000000 ) ) ;
#9083 = CARTESIAN_POINT ( 'NONE',  ( -8.685887942688738761, 506.9948905765655240, -2.449293598294705724E-15 ) ) ;
#9084 = CARTESIAN_POINT ( 'NONE',  ( -162.2727221670389781, 30.52886280891152282, 0.000000000000000000 ) ) ;
#9085 = ADVANCED_FACE ( 'NONE', ( #8893 ), #15302, .F. ) ;
#9086 = CARTESIAN_POINT ( 'NONE',  ( -11.93348319268872970, 439.1823905683720000, -3.332260488124732856 ) ) ;
#9087 = ORIENTED_EDGE ( 'NONE', *, *, #13469, .T. ) ;
#9088 = CARTESIAN_POINT ( 'NONE',  ( -28.68588794268872277, 439.7448905601784759, 19.99999999999999289 ) ) ;
#9089 = VECTOR ( 'NONE', #16649, 1000.000000000000000 ) ;
#9090 = VERTEX_POINT ( 'NONE', #694 ) ;
#9091 = CARTESIAN_POINT ( 'NONE',  ( 5.074999999999999289, 0.000000000000000000, 6.500000000000000888 ) ) ;
#9092 = VERTEX_POINT ( 'NONE', #3813 ) ;
#9093 = ORIENTED_EDGE ( 'NONE', *, *, #5521, .T. ) ;
#9094 = CARTESIAN_POINT ( 'NONE',  ( 5.700000000000000178, 0.000000000000000000, 0.000000000000000000 ) ) ;
#9095 = CARTESIAN_POINT ( 'NONE',  ( -10.20829729246298001, 322.8698905601784759, -7.653668647301794969 ) ) ;
#9096 = AXIS2_PLACEMENT_3D ( 'NONE', #1650, #10061, #6493 ) ;
#9097 = CARTESIAN_POINT ( 'NONE',  ( -16.84014894278198327, 300.1198905683720000, -11.84573899990672707 ) ) ;
#9098 = CARTESIAN_POINT ( 'NONE',  ( -13.20868407381886023, 369.7448905683720568, 6.410867750099229490 ) ) ;
#9099 = CARTESIAN_POINT ( 'NONE',  ( -48.68588794268871567, 391.9948905765656377, 0.000000000000000000 ) ) ;
#9100 = CARTESIAN_POINT ( 'NONE',  ( -16.84014894278199392, 400.1198905683720000, -11.84573899990672707 ) ) ;
#9101 = CARTESIAN_POINT ( 'NONE',  ( -28.68588794268869790, 247.8698905683720000, 16.75240474999999307 ) ) ;
#9102 = CARTESIAN_POINT ( 'NONE',  ( -45.43829269268871940, 403.5573905683721136, -3.332260488124726638 ) ) ;
#9103 = CARTESIAN_POINT ( 'NONE',  ( -47.16347859291444422, 341.3698905765655809, -7.653668647301793193 ) ) ;
#9104 = LINE ( 'NONE', #4131, #17922 ) ;
#9105 = CARTESIAN_POINT ( 'NONE',  ( -40.53162694259543031, 305.1198905683720000, 11.84573899990672885 ) ) ;
#9106 =( LENGTH_UNIT ( ) NAMED_UNIT ( * ) SI_UNIT ( .MILLI., .METRE. ) );
#9107 = CARTESIAN_POINT ( 'NONE',  ( -44.16309181155857999, 455.9948905683720000, 6.410867750099241924 ) ) ;
#9108 = CARTESIAN_POINT ( 'NONE',  ( -42.82802356641968089, 513.2448905765656946, 14.14213562373094923 ) ) ;
#9109 = CARTESIAN_POINT ( 'NONE',  ( -43.20748696942038691, 201.8382954020869420, -3.765466433758053011 ) ) ;
#9110 = CARTESIAN_POINT ( 'NONE',  ( -8.685887942688733432, 456.9948905765656377, -2.449293598294705724E-15 ) ) ;
#9111 = AXIS2_PLACEMENT_3D ( 'NONE', #4824, #11421, #19329 ) ;
#9112 = CARTESIAN_POINT ( 'NONE',  ( -16.84014894278198682, 369.1198905683720000, 11.84573899990672530 ) ) ;
#9113 = CARTESIAN_POINT ( 'NONE',  ( -8.938426032941704028E-16, 600.7448905601785327, 0.000000000000000000 ) ) ;
#9114 = CARTESIAN_POINT ( 'NONE',  ( -17.35679799567831338, 513.8073905601785327, -16.95518130045146421 ) ) ;
#9115 = CARTESIAN_POINT ( 'NONE',  ( -40.53162694259543741, 352.6198905683720000, -11.84573899990672707 ) ) ;
#9116 = ORIENTED_EDGE ( 'NONE', *, *, #18810, .F. ) ;
#9117 = CARTESIAN_POINT ( 'NONE',  ( -13.20868407381887799, 509.4948905683720568, -6.410867750099233042 ) ) ;
#9118 = ORIENTED_EDGE ( 'NONE', *, *, #4262, .T. ) ;
#9119 = CARTESIAN_POINT ( 'NONE',  ( -20.54277306141297998, 585.7448905601785327, -49.33244044267773631 ) ) ;
#9120 = CARTESIAN_POINT ( 'NONE',  ( -13.20868407381886911, 430.9948905683720568, -6.410867750099233042 ) ) ;
#9121 = CARTESIAN_POINT ( 'NONE',  ( 20.42502041961813930, 230.5765313837437418, 49.99999999999999289 ) ) ;
#9122 = CARTESIAN_POINT ( 'NONE',  ( -10.20829729246300488, 517.6198905765656946, -7.653668647301794969 ) ) ;
#9123 = CARTESIAN_POINT ( 'NONE',  ( -42.88789093042844769, 472.9323905683720000, -9.489475012073736337 ) ) ;
#9124 = ORIENTED_EDGE ( 'NONE', *, *, #12814, .T. ) ;
#9125 = CARTESIAN_POINT ( 'NONE',  ( -35.09675569278796559, 475.7448905683720568, 15.47720386886985366 ) ) ;
#9126 = CARTESIAN_POINT ( 'NONE',  ( -21.03221929538689849, 250.3698905601785043, 18.47759065022572500 ) ) ;
#9127 = CARTESIAN_POINT ( 'NONE',  ( -24.70764059509555466, 394.8073905765655809, 19.99999999999998934 ) ) ;
#9128 = CARTESIAN_POINT ( 'NONE',  ( 158.8141120573112630, 628.3356379279406383, 5.000000000000004441 ) ) ;
#9129 = CARTESIAN_POINT ( 'NONE',  ( 125.7989814974898337, 160.1716627696691830, 40.00000000000000000 ) ) ;
#9130 = CARTESIAN_POINT ( 'NONE',  ( 2.416697501590669095, 217.7548513357008630, 45.00000000000000000 ) ) ;
#9131 = CARTESIAN_POINT ( 'NONE',  ( -28.68588794268873698, 548.2448905601784190, 0.000000000000000000 ) ) ;
#9132 = DIRECTION ( 'NONE',  ( 0.9997392892938120612, 0.02283316540262222277, -0.000000000000000000 ) ) ;
#9133 = FILL_AREA_STYLE ('',( #12178 ) ) ;
#9134 = EDGE_CURVE ( 'NONE', #7636, #16109, #15090, .T. ) ;
#9135 = DIRECTION ( 'NONE',  ( -1.000000000000000000, -0.000000000000000000, -0.000000000000000000 ) ) ;
#9136 = CARTESIAN_POINT ( 'NONE',  ( -42.88789093042842637, 286.3073905683720000, 9.489475012073736337 ) ) ;
#9137 = CARTESIAN_POINT ( 'NONE',  ( -36.33955658999050087, 259.1198905601784759, 18.47759065022572500 ) ) ;
#9138 = CYLINDRICAL_SURFACE ( 'NONE', #4367, 4.999999999999990230 ) ;
#9139 = CARTESIAN_POINT ( 'NONE',  ( -19.19641293061498999, 428.8073905683720000, 14.20200298773971426 ) ) ;
#9140 = DIRECTION ( 'NONE',  ( -0.000000000000000000, -1.000000000000000000, -0.000000000000000000 ) ) ;
#9141 = CARTESIAN_POINT ( 'NONE',  ( -16.84014894278197616, 259.1198905683720568, 11.84573899990672530 ) ) ;
#9142 = VERTEX_POINT ( 'NONE', #11929 ) ;
#9143 = CARTESIAN_POINT ( 'NONE',  ( 5.074999999999999289, 7.505553499465139389, 0.000000000000000000 ) ) ;
#9144 = ORIENTED_EDGE ( 'NONE', *, *, #18949, .T. ) ;
#9145 = CARTESIAN_POINT ( 'NONE',  ( -32.01814843081345430, 483.1823905683720000, -16.75240474999999307 ) ) ;
#9146 = ORIENTED_EDGE ( 'NONE', *, *, #18861, .F. ) ;
#9147 = FACE_OUTER_BOUND ( 'NONE', #7566, .T. ) ;
#9148 = CARTESIAN_POINT ( 'NONE',  ( -25.35362745456397704, 241.0573905683720284, -16.75240474999999307 ) ) ;
#9149 = EDGE_LOOP ( 'NONE', ( #1941, #12407, #527, #3774 ) ) ;
#9150 = CARTESIAN_POINT ( 'NONE',  ( -38.17536295476247687, 522.3073905683720568, -14.20200298773971426 ) ) ;
#9151 = FACE_OUTER_BOUND ( 'NONE', #14705, .T. ) ;
#9152 = EDGE_CURVE ( 'NONE', #15607, #8903, #13888, .T. ) ;
#9153 = CARTESIAN_POINT ( 'NONE',  ( -45.64106924314020119, 462.9323905765655809, 11.32908994701042715 ) ) ;
#9154 = DIRECTION ( 'NONE',  ( -0.000000000000000000, -0.000000000000000000, -1.000000000000000000 ) ) ;
#9155 = CARTESIAN_POINT ( 'NONE',  ( -28.68588794268870146, 284.4948905765656377, 19.99999999999999289 ) ) ;
#9156 = CARTESIAN_POINT ( 'NONE',  ( -14.54375231895778064, 453.4948905601784759, -14.14213562373094746 ) ) ;
#9157 = CARTESIAN_POINT ( 'NONE',  ( 10.41669750159067220, 217.7548513357008630, 49.99999999999999289 ) ) ;
#9158 = CARTESIAN_POINT ( 'NONE',  ( -16.84014894278200458, 509.1198905683720568, 11.84573899990672530 ) ) ;
#9159 = SURFACE_STYLE_FILL_AREA ( #18897 ) ;
#9160 = CARTESIAN_POINT ( 'NONE',  ( -40.53162694259542320, 245.1198905683720284, 11.84573899990672885 ) ) ;
#9161 = CARTESIAN_POINT ( 'NONE',  ( -28.68588794268871212, 342.8698905683720000, -16.75240474999999307 ) ) ;
#9162 = DIRECTION ( 'NONE',  ( 0.000000000000000000, -1.000000000000000000, 0.000000000000000000 ) ) ;
#9163 = CARTESIAN_POINT ( 'NONE',  ( -47.16347859291444422, 357.8698905601784759, 7.653668647301805628 ) ) ;
#9164 = ADVANCED_FACE ( 'NONE', ( #3607 ), #2003, .F. ) ;
#9165 = CARTESIAN_POINT ( 'NONE',  ( -13.20868407381886200, 388.2448905683720000, 6.410867750099229490 ) ) ;
#9166 = CARTESIAN_POINT ( 'NONE',  ( -44.16309181155859420, 534.7448905683720568, -6.410867750099231266 ) ) ;
#9167 = CARTESIAN_POINT ( 'NONE',  ( -8.685887942688724550, 391.9323905601784759, 3.978247347593161010 ) ) ;
#9168 = EDGE_LOOP ( 'NONE', ( #12945, #16014, #14414 ) ) ;
#9169 = CARTESIAN_POINT ( 'NONE',  ( -17.35679799567828141, 228.5573905765656093, -16.95518130045146421 ) ) ;
#9170 = ORIENTED_EDGE ( 'NONE', *, *, #11264, .T. ) ;
#9171 = ORIENTED_EDGE ( 'NONE', *, *, #1780, .T. ) ;
#9172 = CARTESIAN_POINT ( 'NONE',  ( -45.43829269268872650, 515.0573905683720568, -3.332260488124726194 ) ) ;
#9173 = DIRECTION ( 'NONE',  ( -1.191790137725560488E-16, 1.000000000000000000, -0.000000000000000000 ) ) ;
#9174 = ORIENTED_EDGE ( 'NONE', *, *, #9004, .T. ) ;
#9175 = ADVANCED_FACE ( 'NONE', ( #8789 ), #1898, .F. ) ;
#9176 = CARTESIAN_POINT ( 'NONE',  ( -13.20868407381885135, 309.7448905683720568, 6.410867750099229490 ) ) ;
#9177 = VERTEX_POINT ( 'NONE', #18522 ) ;
#9178 = CARTESIAN_POINT ( 'NONE',  ( -42.88789093042843348, 344.8073905683719431, 9.489475012073736337 ) ) ;
#9179 = CARTESIAN_POINT ( 'NONE',  ( -40.53162694259543741, 355.1198905683720568, 11.84573899990672885 ) ) ;
#9180 = CARTESIAN_POINT ( 'NONE',  ( -17.35679799567828496, 285.4323905765656377, 16.95518130045146421 ) ) ;
#9181 = CARTESIAN_POINT ( 'NONE',  ( -28.68588794268873343, 499.4948905765656377, -19.99999999999999289 ) ) ;
#9182 = CARTESIAN_POINT ( 'NONE',  ( -16.84014894278197261, 247.6198905683720284, 11.84573899990672530 ) ) ;
#9183 = CARTESIAN_POINT ( 'NONE',  ( -19.81321358049341086, 224.0162454934389586, -17.97266195050653081 ) ) ;
#9184 =( BOUNDED_CURVE ( )  B_SPLINE_CURVE ( 2, ( #6498, #6106, #1658, #9356, #12718, #255, #10972, #12614, #13227, #9747, #31, #17965, #11482, #17581, #8227, #21330, #14856 ),
 .UNSPECIFIED., .F., .T. ) 
 B_SPLINE_CURVE_WITH_KNOTS ( ( 3, 2, 2, 2, 2, 2, 2, 2, 3 ),
 ( 0.2656250000000002220, 0.2675781250000002220, 0.2695312500000001665, 0.2714843750000001665, 0.2734375000000001110, 0.2753906250000001110, 0.2773437500000001110, 0.2792968750000000555, 0.2812500000000000555 ),
 .UNSPECIFIED. ) 
 CURVE ( )  GEOMETRIC_REPRESENTATION_ITEM ( )  RATIONAL_B_SPLINE_CURVE ( ( 0.9999999999999977796, 0.9807852804032326510, 1.000000000000000000, 0.9807852804032304306, 1.000000000000000000, 0.9807852804032304306, 1.000000000000000000, 0.9807852804032304306, 1.000000000000000000, 0.9807852804032304306, 1.000000000000000000, 0.9807852804032304306, 1.000000000000000000, 0.9807852804032304306, 1.000000000000000000, 0.9807852804032298755, 1.000000000000000444 ) ) 
 REPRESENTATION_ITEM ( '' )  );
#9185 = CARTESIAN_POINT ( 'NONE',  ( -14.48388495494900496, 401.3073905683720568, -9.489475012073736337 ) ) ;
#9186 = VECTOR ( 'NONE', #17552, 1000.000000000000000 ) ;
#9187 = DIRECTION ( 'NONE',  ( -1.000000000000000000, 0.000000000000000000, 0.000000000000000000 ) ) ;
#9188 = PLANE ( 'NONE',  #3134 ) ;
#9189 = CARTESIAN_POINT ( 'NONE',  ( -48.68588794268860198, 246.9323905601784475, -3.978247347593371508 ) ) ;
#9190 = AXIS2_PLACEMENT_3D ( 'NONE', #19919, #19699, #3480 ) ;
#9191 = CARTESIAN_POINT ( 'NONE',  ( -19.19641293061498999, 447.3073905683720568, 14.20200298773971426 ) ) ;
#9192 = ORIENTED_EDGE ( 'NONE', *, *, #19162, .T. ) ;
#9193 = CARTESIAN_POINT ( 'NONE',  ( -47.16347859291445133, 437.8698905601784759, 7.653668647301805628 ) ) ;
#9194 = ORIENTED_EDGE ( 'NONE', *, *, #20063, .T. ) ;
#9195 = EDGE_LOOP ( 'NONE', ( #14036, #4070 ) ) ;
#9196 = ORIENTED_EDGE ( 'NONE', *, *, #18597, .T. ) ;
#9197 = DIRECTION ( 'NONE',  ( -1.000000000000000000, 0.000000000000000000, 0.000000000000000000 ) ) ;
#9198 = CARTESIAN_POINT ( 'NONE',  ( -11.73070664223724080, 321.3073905601784759, 11.32908994701042005 ) ) ;
#9199 = CARTESIAN_POINT ( 'NONE',  ( -19.19641293061498288, 361.9323905683720568, -14.20200298773971603 ) ) ;
#9200 = AXIS2_PLACEMENT_3D ( 'NONE', #6345, #14277, #7858 ) ;
#9201 = CARTESIAN_POINT ( 'NONE',  ( 0.4033376246892552697, -7.198601258566911021, 0.5316568767328686551 ) ) ;
#9202 = CARTESIAN_POINT ( 'NONE',  ( -14.54375231895778953, 518.2448905765656946, -14.14213562373094746 ) ) ;
#9203 = CARTESIAN_POINT ( 'NONE',  ( -11.93348319268872615, 409.1823905683720568, -3.332260488124732856 ) ) ;
#9204 = CARTESIAN_POINT ( 'NONE',  ( -42.88789093042841927, 244.4323905683720284, -9.489475012073736337 ) ) ;
#9205 = ADVANCED_FACE ( 'NONE', ( #3708 ), #9317, .T. ) ;
#9206 = CARTESIAN_POINT ( 'NONE',  ( -28.68588794268871567, 396.3698905683720000, 16.75240474999999307 ) ) ;
#9207 = CONTEXT_DEPENDENT_SHAPE_REPRESENTATION ( #1573, #6470 ) ;
#9208 = EDGE_CURVE ( 'NONE', #8877, #13368, #10663, .T. ) ;
#9209 = VECTOR ( 'NONE', #5785, 1000.000000000000000 ) ;
#9210 = CARTESIAN_POINT ( 'NONE',  ( -11.73070664223724968, 347.9323905765655809, -11.32908994701042715 ) ) ;
#9211 = DIRECTION ( 'NONE',  ( 0.000000000000000000, 0.000000000000000000, 1.000000000000000000 ) ) ;
#9212 = CARTESIAN_POINT ( 'NONE',  ( -38.17536295476244135, 305.4323905683720000, 14.20200298773971781 ) ) ;
#9213 = CARTESIAN_POINT ( 'NONE',  ( -14.48388495494901029, 461.3073905683720568, -9.489475012073736337 ) ) ;
#9214 = LINE ( 'NONE', #4461, #14080 ) ;
#9215 = CARTESIAN_POINT ( 'NONE',  ( 0.4037800551813744421, 7.199367570657605242, 0.5303295852573141067 ) ) ;
#9216 = FACE_OUTER_BOUND ( 'NONE', #9916, .T. ) ;
#9217 = EDGE_CURVE ( 'NONE', #10520, #13969, #18838, .T. ) ;
#9218 = VECTOR ( 'NONE', #616, 1000.000000000000000 ) ;
#9219 = CARTESIAN_POINT ( 'NONE',  ( -14.48388495494900141, 371.3073905683720568, -9.489475012073736337 ) ) ;
#9220 = CARTESIAN_POINT ( 'NONE',  ( -40.53162694259545162, 495.1198905683720000, 11.84573899990672885 ) ) ;
#9221 = CARTESIAN_POINT ( 'NONE',  ( -10.20829729246300310, 502.8698905601784759, -7.653668647301794969 ) ) ;
#9222 = CARTESIAN_POINT ( 'NONE',  ( -38.17536295476244135, 325.4323905683720000, 14.20200298773971781 ) ) ;
#9223 = EDGE_CURVE ( 'NONE', #11679, #12774, #9104, .T. ) ;
#9224 = AXIS2_PLACEMENT_3D ( 'NONE', #20560, #10810, #2392 ) ;
#9225 = VERTEX_POINT ( 'NONE', #19275 ) ;
#9226 = CARTESIAN_POINT ( 'NONE',  ( -13.20868407381887621, 508.2448905683720568, 6.410867750099229490 ) ) ;
#9227 = PRODUCT_DEFINITION_SHAPE ( 'NONE', 'NONE',  #19867 ) ;
#9228 = ORIENTED_EDGE ( 'NONE', *, *, #2966, .T. ) ;
#9229 = DIRECTION ( 'NONE',  ( 0.000000000000000000, 0.000000000000000000, 1.000000000000000000 ) ) ;
#9230 = CARTESIAN_POINT ( 'NONE',  ( -22.27502019258949417, 432.2448905683720000, -15.47720386886985544 ) ) ;
#9231 = DIRECTION ( 'NONE',  ( -1.000000000000000000, 0.000000000000000000, 0.000000000000000000 ) ) ;
#9232 = CARTESIAN_POINT ( 'NONE',  ( 158.8141120573112630, 610.7448905601785327, 0.000000000000000000 ) ) ;
#9233 = CARTESIAN_POINT ( 'NONE',  ( -19.19641293061499354, 467.3073905683721136, 14.20200298773971426 ) ) ;
#9234 = ORIENTED_EDGE ( 'NONE', *, *, #16099, .F. ) ;
#9235 = CARTESIAN_POINT ( 'NONE',  ( -11.93348319268873325, 458.5573905683720568, 3.332260488124728859 ) ) ;
#9236 = CARTESIAN_POINT ( 'NONE',  ( -48.68588794268878672, 247.5573905601784759, 3.978247347592954952 ) ) ;
#9237 = EDGE_CURVE ( 'NONE', #16482, #11027, #17234, .T. ) ;
#9238 = VECTOR ( 'NONE', #13807, 1000.000000000000000 ) ;
#9239 = CARTESIAN_POINT ( 'NONE',  ( -14.54375231895777532, 408.2448905765655809, -14.14213562373094746 ) ) ;
#9240 = DIRECTION ( 'NONE',  ( 0.000000000000000000, 0.000000000000000000, -1.000000000000000000 ) ) ;
#9241 = CARTESIAN_POINT ( 'NONE',  ( 6.416697501590670427, 217.7548513357008630, 45.00000000000000000 ) ) ;
#9242 = CARTESIAN_POINT ( 'NONE',  ( 0.06682554136337785777, 4.993536075455418555, -4.350941807883112133 ) ) ;
#9243 = CARTESIAN_POINT ( 'NONE',  ( -54.57497958038185715, 160.1716627696692683, 25.00000000000000000 ) ) ;
#9244 = VECTOR ( 'NONE', #1849, 1000.000000000000000 ) ;
#9245 = CARTESIAN_POINT ( 'NONE',  ( -49.57497958038186425, 230.5765313837437418, 49.99999999999999289 ) ) ;
#9246 = CARTESIAN_POINT ( 'NONE',  ( -28.68588794268872988, 47.23886018424757083, -49.60091809715359545 ) ) ;
#9247 = CARTESIAN_POINT ( 'NONE',  ( -24.70764059509555466, 344.4323905601784759, -19.99999999999999289 ) ) ;
#9248 = CARTESIAN_POINT ( 'NONE',  ( -17.35679799567828496, 253.8073905601785043, -16.95518130045146421 ) ) ;
#9249 = CARTESIAN_POINT ( 'NONE',  ( -28.68588794268871922, 404.4948905765656377, 19.99999999999999289 ) ) ;
#9250 = CARTESIAN_POINT ( 'NONE',  ( -28.68588794268871922, 427.8698905683720568, 16.75240474999999307 ) ) ;
#9251 = DIRECTION ( 'NONE',  ( -0.000000000000000000, -0.000000000000000000, -1.000000000000000000 ) ) ;
#9252 = CARTESIAN_POINT ( 'NONE',  ( -35.09675569278793716, 247.2448905683720000, 15.47720386886985366 ) ) ;
#9253 = ORIENTED_EDGE ( 'NONE', *, *, #8013, .T. ) ;
#9254 = ORIENTED_EDGE ( 'NONE', *, *, #219, .T. ) ;
#9255 = DIRECTION ( 'NONE',  ( -1.191790137725560488E-16, 1.000000000000000000, -0.000000000000000000 ) ) ;
#9256 = ORIENTED_EDGE ( 'NONE', *, *, #20274, .T. ) ;
#9257 = CARTESIAN_POINT ( 'NONE',  ( -11.93348319268873325, 460.6823905683720568, -3.332260488124732856 ) ) ;
#9258 = ORIENTED_EDGE ( 'NONE', *, *, #17558, .T. ) ;
#9259 = ADVANCED_FACE ( 'NONE', ( #15725 ), #10721, .F. ) ;
#9260 = CARTESIAN_POINT ( 'NONE',  ( -35.09675569278793006, 231.9948905683720284, -15.47720386886985544 ) ) ;
#9261 = VERTEX_POINT ( 'NONE', #19065 ) ;
#9262 = CARTESIAN_POINT ( 'NONE',  ( -11.93348319268874036, 518.5573905683720568, 3.332260488124728859 ) ) ;
#9263 = PLANE ( 'NONE',  #7623 ) ;
#9264 = CARTESIAN_POINT ( 'NONE',  ( -32.66413529028189089, 464.1823905765656377, 19.99999999999999289 ) ) ;
#9265 = CARTESIAN_POINT ( 'NONE',  ( 0.4033376246892542705, -7.198601258566906580, 0.5316568767328695433 ) ) ;
#9266 = CYLINDRICAL_SURFACE ( 'NONE', #9424, 19.99999999999999645 ) ;
#9267 = CARTESIAN_POINT ( 'NONE',  ( 0.000000000000000000, 0.000000000000000000, 60.00000000000000000 ) ) ;
#9268 = CARTESIAN_POINT ( 'NONE',  ( 158.8141120573112630, 10.52886280891152104, -10.00000000000000888 ) ) ;
#9269 = VECTOR ( 'NONE', #16864, 1000.000000000000000 ) ;
#9270 = CARTESIAN_POINT ( 'NONE',  ( -11.93348319268873858, 510.6823905683720000, -3.332260488124732856 ) ) ;
#9271 = CARTESIAN_POINT ( 'NONE',  ( -13.68588794268869435, 193.9102039777116602, 1.836970198721029983E-15 ) ) ;
#9272 = CARTESIAN_POINT ( 'NONE',  ( -28.68588794268870146, 231.3698905683720284, -16.75240474999999307 ) ) ;
#9273 = CARTESIAN_POINT ( 'NONE',  ( -16.84014894278198327, 339.1198905683720568, 11.84573899990672530 ) ) ;
#9274 = CARTESIAN_POINT ( 'NONE',  ( -17.35679799567830273, 470.6823905601784759, 16.95518130045146421 ) ) ;
#9275 = LINE ( 'NONE', #15891, #5741 ) ;
#9276 = EDGE_CURVE ( 'NONE', #1881, #17507, #10618, .T. ) ;
#9277 = CARTESIAN_POINT ( 'NONE',  ( -35.09675569278794427, 381.9948905683720568, -15.47720386886985544 ) ) ;
#9278 = CARTESIAN_POINT ( 'NONE',  ( -47.06209031768872819, 536.3073905642752379, 0.000000000000000000 ) ) ;
#9279 = CARTESIAN_POINT ( 'NONE',  ( -10.20829729246298889, 391.6198905601784759, 7.653668647301790529 ) ) ;
#9280 = AXIS2_PLACEMENT_3D ( 'NONE', #13487, #20082, #3734 ) ;
#9281 = LINE ( 'NONE', #12858, #2544 ) ;
#9282 = ORIENTED_EDGE ( 'NONE', *, *, #17736, .T. ) ;
#9283 = ORIENTED_EDGE ( 'NONE', *, *, #14181, .F. ) ;
#9284 = CARTESIAN_POINT ( 'NONE',  ( -42.88789093042845479, 514.4323905683720568, -9.489475012073736337 ) ) ;
#9285 = CARTESIAN_POINT ( 'NONE',  ( -74.06037022053952512, 10.52886280891152104, 40.00000000000000000 ) ) ;
#9286 = EDGE_LOOP ( 'NONE', ( #17430, #9515, #2404, #3390 ) ) ;
#9287 = CARTESIAN_POINT ( 'NONE',  ( -44.16309181155856578, 294.7448905683720568, -6.410867750099231266 ) ) ;
#9288 = ORIENTED_EDGE ( 'NONE', *, *, #3168, .F. ) ;
#9289 = CARTESIAN_POINT ( 'NONE',  ( -42.88789093042842637, 324.8073905683720000, 9.489475012073736337 ) ) ;
#9290 = EDGE_CURVE ( 'NONE', #13610, #19679, #3767, .T. ) ;
#9291 = CARTESIAN_POINT ( 'NONE',  ( -47.16347859291443712, 272.6198905765655809, 7.653668647301805628 ) ) ;
#9292 = FACE_OUTER_BOUND ( 'NONE', #5819, .T. ) ;
#9293 = CARTESIAN_POINT ( 'NONE',  ( -11.93348319268870661, 248.5573905683719715, 3.332260488124728859 ) ) ;
#9294 = APPLICATION_CONTEXT ( 'automotive_design' ) ;
#9295 = CARTESIAN_POINT ( 'NONE',  ( -13.20868407381886378, 390.9948905683720568, -6.410867750099233042 ) ) ;
#9296 = CARTESIAN_POINT ( 'NONE',  ( 30.42502041961814996, 180.1716627696692967, -40.00000000000000000 ) ) ;
#9297 = CARTESIAN_POINT ( 'NONE',  ( 18.55315245287936321, 213.9102039777116602, 0.000000000000000000 ) ) ;
#9298 = CYLINDRICAL_SURFACE ( 'NONE', #10451, 4.999999999999990230 ) ;
#9299 = EDGE_CURVE ( 'NONE', #9623, #12668, #17652, .T. ) ;
#9300 = EDGE_CURVE ( 'NONE', #7992, #13900, #6529, .T. ) ;
#9301 = CARTESIAN_POINT ( 'NONE',  ( -38.17536295476245556, 445.4323905683720568, 14.20200298773971781 ) ) ;
#9302 = VERTEX_POINT ( 'NONE', #12682 ) ;
#9303 = CARTESIAN_POINT ( 'NONE',  ( -47.16347859291445843, 456.6198905601784759, -7.653668647301793193 ) ) ;
#9304 = VERTEX_POINT ( 'NONE', #1123 ) ;
#9305 = ORIENTED_EDGE ( 'NONE', *, *, #12363, .T. ) ;
#9306 = CARTESIAN_POINT ( 'NONE',  ( -28.68588794268875120, 585.7448905601785327, 0.000000000000000000 ) ) ;
#9307 = CARTESIAN_POINT ( 'NONE',  ( -48.68588794268870146, 317.5573905601784759, 3.978247347593168115 ) ) ;
#9308 = AXIS2_PLACEMENT_3D ( 'NONE', #8519, #18257, #6789 ) ;
#9309 = CARTESIAN_POINT ( 'NONE',  ( -45.43829269268871229, 365.0573905683720568, -3.332260488124726638 ) ) ;
#9310 = CARTESIAN_POINT ( 'NONE',  ( 2.416697501590669095, 217.7548513357008630, 49.99999999999999289 ) ) ;
#9311 = CARTESIAN_POINT ( 'NONE',  ( -8.685887942688738761, 496.9948905765655809, -2.449293598294705724E-15 ) ) ;
#9312 = CARTESIAN_POINT ( 'NONE',  ( -13.20868407381886378, 389.4948905683720000, -6.410867750099233042 ) ) ;
#9313 = CARTESIAN_POINT ( 'NONE',  ( -22.27502019258947286, 242.2448905683720000, -15.47720386886985544 ) ) ;
#9314 = CARTESIAN_POINT ( 'NONE',  ( -13.20868407381886556, 409.4948905683720000, -6.410867750099233042 ) ) ;
#9315 =( BOUNDED_CURVE ( )  B_SPLINE_CURVE ( 2, ( #12304, #5915, #10560, #18894, #2576, #1073, #12413, #4080, #20854, #19006, #10666, #2683, #9156, #12526, #15779, #13828, #17285 ),
 .UNSPECIFIED., .F., .T. ) 
 B_SPLINE_CURVE_WITH_KNOTS ( ( 3, 2, 2, 2, 2, 2, 2, 2, 3 ),
 ( 0.2500000000000002220, 0.2519531250000002220, 0.2539062500000002220, 0.2558593750000002220, 0.2578125000000002220, 0.2597656250000002220, 0.2617187500000002220, 0.2636718750000002220, 0.2656250000000002220 ),
 .UNSPECIFIED. ) 
 CURVE ( )  GEOMETRIC_REPRESENTATION_ITEM ( )  RATIONAL_B_SPLINE_CURVE ( ( 0.9999999999999977796, 0.9807852804032326510, 1.000000000000000000, 0.9807852804032304306, 1.000000000000000000, 0.9807852804032304306, 1.000000000000000000, 0.9807852804032304306, 1.000000000000000000, 0.9807852804032304306, 1.000000000000000000, 0.9807852804032304306, 1.000000000000000000, 0.9807852804032304306, 1.000000000000000000, 0.9807852804032282101, 1.000000000000002220 ) ) 
 REPRESENTATION_ITEM ( '' )  );
#9316 = CARTESIAN_POINT ( 'NONE',  ( -24.70764059509554755, 334.8073905765656377, 19.99999999999998934 ) ) ;
#9317 = CYLINDRICAL_SURFACE ( 'NONE', #671, 53.46661168214943416 ) ;
#9318 = CARTESIAN_POINT ( 'NONE',  ( -13.20868407381885135, 308.2448905683720000, 6.410867750099229490 ) ) ;
#9319 =( NAMED_UNIT ( * ) PLANE_ANGLE_UNIT ( ) SI_UNIT ( $, .RADIAN. ) );
#9320 = CARTESIAN_POINT ( 'NONE',  ( -14.48388495494900852, 451.3073905683721136, -9.489475012073736337 ) ) ;
#9321 = CARTESIAN_POINT ( 'NONE',  ( -28.68588794268874409, 608.2448905601786464, 0.000000000000000000 ) ) ;
#9322 = CARTESIAN_POINT ( 'NONE',  ( 5.074999999999999289, -3.752776749732576800, -6.500000000000000000 ) ) ;
#9323 = CARTESIAN_POINT ( 'NONE',  ( 5.674999999999999822, 0.000000000000000000, 0.000000000000000000 ) ) ;
#9324 = CARTESIAN_POINT ( 'NONE',  ( -45.43829269268871229, 365.3698905683720568, 0.000000000000000000 ) ) ;
#9325 = CARTESIAN_POINT ( 'NONE',  ( -19.19641293061500065, 500.4323905683721136, -14.20200298773971603 ) ) ;
#9326 = CARTESIAN_POINT ( 'NONE',  ( -8.685887942688740537, 502.5573905601785896, -3.978247347593165895 ) ) ;
#9327 = CARTESIAN_POINT ( 'NONE',  ( -25.35362745456398770, 321.0573905683720568, -16.75240474999999307 ) ) ;
#9328 = EDGE_LOOP ( 'NONE', ( #16776, #927, #2141, #4423, #10880 ) ) ;
#9329 = CARTESIAN_POINT ( 'NONE',  ( -47.16347859291446554, 526.6198905601784190, -7.653668647301793193 ) ) ;
#9330 = ORIENTED_EDGE ( 'NONE', *, *, #14142, .F. ) ;
#9331 = DIRECTION ( 'NONE',  ( 0.000000000000000000, 1.000000000000000000, 0.000000000000000000 ) ) ;
#9332 = CARTESIAN_POINT ( 'NONE',  ( -38.17536295476246266, 423.8073905683720568, -14.20200298773971426 ) ) ;
#9333 = DIRECTION ( 'NONE',  ( -1.250996701150283068E-16, 1.000000000000000000, 0.000000000000000000 ) ) ;
#9334 = DIRECTION ( 'NONE',  ( 0.000000000000000000, 0.000000000000000000, -1.000000000000000000 ) ) ;
#9335 = CARTESIAN_POINT ( 'NONE',  ( -22.27502019258948707, 436.9948905683720568, 15.47720386886985189 ) ) ;
#9336 = ORIENTED_EDGE ( 'NONE', *, *, #17938, .T. ) ;
#9337 = CARTESIAN_POINT ( 'NONE',  ( -22.27502019258949773, 470.7448905683720568, -15.47720386886985544 ) ) ;
#9338 = CARTESIAN_POINT ( 'NONE',  ( 0.000000000000000000, 0.000000000000000000, 0.000000000000000000 ) ) ;
#9339 = PLANE ( 'NONE',  #4809 ) ;
#9340 = ADVANCED_FACE ( 'NONE', ( #12469, #4352 ), #10936, .F. ) ;
#9341 = VECTOR ( 'NONE', #2006, 1000.000000000000000 ) ;
#9342 = CARTESIAN_POINT ( 'NONE',  ( -8.685887942688726326, 397.3073905765656946, -3.978247347593165895 ) ) ;
#9343 = CARTESIAN_POINT ( 'NONE',  ( -14.54375231895776110, 278.2448905765655809, -14.14213562373094746 ) ) ;
#9344 = CARTESIAN_POINT ( 'NONE',  ( -28.68588794268873698, 548.2448905601784190, 0.000000000000000000 ) ) ;
#9345 = CARTESIAN_POINT ( 'NONE',  ( -162.2727221670389781, 10.52886280891152104, 4.999999999999990230 ) ) ;
#9346 = CARTESIAN_POINT ( 'NONE',  ( -48.68588794268871567, 441.9948905765656377, 0.000000000000000000 ) ) ;
#9347 = EDGE_CURVE ( 'NONE', #12450, #12520, #18617, .T. ) ;
#9348 = EDGE_CURVE ( 'NONE', #14679, #3567, #7795, .T. ) ;
#9349 = AXIS2_PLACEMENT_3D ( 'NONE', #11764, #16964, #3653 ) ;
#9350 = CARTESIAN_POINT ( 'NONE',  ( -28.68588794268872633, 378.8848358243226357, 0.000000000000000000 ) ) ;
#9351 = VECTOR ( 'NONE', #7588, 1000.000000000000000 ) ;
#9352 = CYLINDRICAL_SURFACE ( 'NONE', #1813, 20.00000000000000355 ) ;
#9353 = CARTESIAN_POINT ( 'NONE',  ( -38.88879370254166190, 223.9102039777117170, 16.61907291475590043 ) ) ;
#9354 = AXIS2_PLACEMENT_3D ( 'NONE', #1996, #6940, #8564 ) ;
#9355 = CARTESIAN_POINT ( 'NONE',  ( -10.20829729246297291, 241.6198905601784759, 7.653668647301790529 ) ) ;
#9356 = CARTESIAN_POINT ( 'NONE',  ( -11.73070664223725679, 451.3073905601784759, 11.32908994701042005 ) ) ;
#9357 = CARTESIAN_POINT ( 'NONE',  ( -28.68588794268872277, 422.8698905683720568, -16.75240474999999307 ) ) ;
#9358 = DIRECTION ( 'NONE',  ( -1.000000000000000000, 0.000000000000000000, 0.000000000000000000 ) ) ;
#9359 = VECTOR ( 'NONE', #20529, 1000.000000000000000 ) ;
#9360 = CARTESIAN_POINT ( 'NONE',  ( -16.84014894278197261, 249.1198905683720284, 11.84573899990672530 ) ) ;
#9361 = EDGE_CURVE ( 'NONE', #18908, #6352, #17758, .T. ) ;
#9362 = ORIENTED_EDGE ( 'NONE', *, *, #4137, .F. ) ;
#9363 = ORIENTED_EDGE ( 'NONE', *, *, #5300, .T. ) ;
#9364 = CARTESIAN_POINT ( 'NONE',  ( -40.01497788969915348, 480.4323905765656377, -16.95518130045146421 ) ) ;
#9365 = ORIENTED_EDGE ( 'NONE', *, *, #15650, .T. ) ;
#9366 = CARTESIAN_POINT ( 'NONE',  ( -35.09675569278796559, 467.2448905683720568, 15.47720386886985366 ) ) ;
#9367 = CARTESIAN_POINT ( 'NONE',  ( -24.70764059509554755, 229.1823905765656377, -19.99999999999999289 ) ) ;
#9368 = VECTOR ( 'NONE', #2876, 1000.000000000000000 ) ;
#9369 = AXIS2_PLACEMENT_3D ( 'NONE', #15623, #15308, #495 ) ;
#9370 = ORIENTED_EDGE ( 'NONE', *, *, #16824, .F. ) ;
#9371 = CARTESIAN_POINT ( 'NONE',  ( -8.685887942688722774, 362.2448905601784190, -2.449293598294705724E-15 ) ) ;
#9372 = VERTEX_POINT ( 'NONE', #23 ) ;
#9373 = CARTESIAN_POINT ( 'NONE',  ( -19.19641293061499709, 517.3073905683720568, 14.20200298773971426 ) ) ;
#9374 = DIRECTION ( 'NONE',  ( -1.191790137725560488E-16, 1.000000000000000000, -0.000000000000000000 ) ) ;
#9375 = CARTESIAN_POINT ( 'NONE',  ( -17.35679799567830983, 458.5573905765656377, -16.95518130045146421 ) ) ;
#9376 = CARTESIAN_POINT ( 'NONE',  ( -28.68588794268875475, 600.7448905601785327, 0.000000000000000000 ) ) ;
#9377 = LINE ( 'NONE', #15013, #7006 ) ;
#9378 = CARTESIAN_POINT ( 'NONE',  ( 1.521271173268723212E-15, -5.309483803148806302, -3.803704290982254932 ) ) ;
#9379 = DIRECTION ( 'NONE',  ( 0.000000000000000000, 0.000000000000000000, -1.000000000000000000 ) ) ;
#9380 = CARTESIAN_POINT ( 'NONE',  ( -11.73821085826490851, 223.9102039777117739, 10.74164566205277715 ) ) ;
#9381 = CARTESIAN_POINT ( 'NONE',  ( -13.20868407381884424, 228.2448905683720568, 6.410867750099229490 ) ) ;
#9382 = CARTESIAN_POINT ( 'NONE',  ( -38.17536295476244845, 313.8073905683720000, -14.20200298773971426 ) ) ;
#9383 = FACE_OUTER_BOUND ( 'NONE', #17142, .T. ) ;
#9384 = CARTESIAN_POINT ( 'NONE',  ( 0.4053525175235891398, 3.145852061455925774, 6.499999999999999112 ) ) ;
#9385 = VECTOR ( 'NONE', #17094, 1000.000000000000000 ) ;
#9386 = CARTESIAN_POINT ( 'NONE',  ( -28.68588794268870856, 317.8698905683720000, 16.75240474999999307 ) ) ;
#9387 = CARTESIAN_POINT ( 'NONE',  ( -42.88789093042843348, 374.8073905683720568, 9.489475012073736337 ) ) ;
#9388 = CARTESIAN_POINT ( 'NONE',  ( -14.48388495494901740, 529.4323905683720568, 9.489475012073731008 ) ) ;
#9389 = CARTESIAN_POINT ( 'NONE',  ( -32.66413529028188378, 395.0573905601784190, -19.99999999999999289 ) ) ;
#9390 = EDGE_LOOP ( 'NONE', ( #11197, #16654, #17322, #11352 ) ) ;
#9391 = ORIENTED_EDGE ( 'NONE', *, *, #4262, .F. ) ;
#9392 = VERTEX_POINT ( 'NONE', #8108 ) ;
#9393 = CARTESIAN_POINT ( 'NONE',  ( -42.88789093042844769, 496.3073905683720568, 9.489475012073736337 ) ) ;
#9394 = CARTESIAN_POINT ( 'NONE',  ( 107.6674317086782935, 187.4856410316723441, -40.00000000000000000 ) ) ;
#9395 = ORIENTED_EDGE ( 'NONE', *, *, #11250, .T. ) ;
#9396 = CARTESIAN_POINT ( 'NONE',  ( -45.43829269268870519, 295.0573905683720000, -3.332260488124726638 ) ) ;
#9397 = CARTESIAN_POINT ( 'NONE',  ( -32.01814843081344009, 321.6823905683720568, -16.75240474999999307 ) ) ;
#9398 = AXIS2_PLACEMENT_3D ( 'NONE', #10969, #11394, #2875 ) ;
#9399 = EDGE_CURVE ( 'NONE', #13969, #20205, #21040, .T. ) ;
#9400 = CARTESIAN_POINT ( 'NONE',  ( -11.73070664223723547, 266.0573905765655809, 11.32908994701042005 ) ) ;
#9401 = DIRECTION ( 'NONE',  ( -1.000000000000000000, 0.000000000000000000, 0.000000000000000000 ) ) ;
#9402 = DIRECTION ( 'NONE',  ( 1.000000000000000000, 0.000000000000000000, 0.000000000000000000 ) ) ;
#9403 = CARTESIAN_POINT ( 'NONE',  ( -40.53162694259544452, 394.1198905683720000, -11.84573899990672707 ) ) ;
#9404 = DIRECTION ( 'NONE',  ( -1.000000000000000000, 0.000000000000000000, 0.000000000000000000 ) ) ;
#9405 = CARTESIAN_POINT ( 'NONE',  ( -28.68588794268874054, 573.2448905601785327, 0.000000000000000000 ) ) ;
#9406 = PRODUCT_DEFINITION_SHAPE ( 'NONE', 'NONE',  #21402 ) ;
#9407 = EDGE_CURVE ( 'NONE', #11603, #827, #5852, .T. ) ;
#9408 = CIRCLE ( 'NONE', #15654, 6.500000000000000888 ) ;
#9409 = CARTESIAN_POINT ( 'NONE',  ( -11.73070664223723547, 243.1823905601784759, -11.32908994701042538 ) ) ;
#9410 = CARTESIAN_POINT ( 'NONE',  ( -16.84014894278199748, 447.6198905683720568, 11.84573899990672530 ) ) ;
#9411 = LINE ( 'NONE', #1413, #12227 ) ;
#9412 = ORIENTED_EDGE ( 'NONE', *, *, #8010, .T. ) ;
#9413 = CARTESIAN_POINT ( 'NONE',  ( -11.73070664223725679, 451.3073905601785327, 11.32908994701042005 ) ) ;
#9414 = ORIENTED_EDGE ( 'NONE', *, *, #16475, .T. ) ;
#9415 = ORIENTED_EDGE ( 'NONE', *, *, #6445, .T. ) ;
#9416 = EDGE_LOOP ( 'NONE', ( #17216, #3491, #18222, #8373 ) ) ;
#9417 = CARTESIAN_POINT ( 'NONE',  ( -21.03221929538690560, 320.3698905601785327, 18.47759065022572500 ) ) ;
#9418 = DIRECTION ( 'NONE',  ( 0.000000000000000000, 0.000000000000000000, 1.000000000000000000 ) ) ;
#9419 = CARTESIAN_POINT ( 'NONE',  ( -45.43829269268871229, 355.0573905683720568, -3.332260488124726638 ) ) ;
#9420 = DIRECTION ( 'NONE',  ( 1.000000000000000000, 0.000000000000000000, 0.000000000000000000 ) ) ;
#9421 = CARTESIAN_POINT ( 'NONE',  ( -11.73070664223726389, 506.0573905765656377, 11.32908994701042005 ) ) ;
#9422 = CARTESIAN_POINT ( 'NONE',  ( -14.48388495494900141, 379.8073905683720568, -9.489475012073736337 ) ) ;
#9423 = CARTESIAN_POINT ( 'NONE',  ( 81.24038404635965094, 30.52886280891152282, -131.1729372809869005 ) ) ;
#9424 = AXIS2_PLACEMENT_3D ( 'NONE', #4617, #3000, #2901 ) ;
#9425 = CARTESIAN_POINT ( 'NONE',  ( -11.93348319268872615, 399.1823905683720568, -3.332260488124732856 ) ) ;
#9426 = EDGE_CURVE ( 'NONE', #19050, #12773, #20408, .T. ) ;
#9427 = CARTESIAN_POINT ( 'NONE',  ( -45.64106924314018698, 331.0573905765655809, -11.32908994701042715 ) ) ;
#9428 = DIRECTION ( 'NONE',  ( 0.000000000000000000, 0.000000000000000000, 1.000000000000000000 ) ) ;
#9429 = CARTESIAN_POINT ( 'NONE',  ( -13.20868407381885490, 309.4948905683720568, -6.410867750099233042 ) ) ;
#9430 = CARTESIAN_POINT ( 'NONE',  ( -25.35362745456399125, 448.1823905683719431, 16.75240474999998952 ) ) ;
#9431 = CARTESIAN_POINT ( 'NONE',  ( 91.21585410611801592, 31.85652257517428865, 40.00000000000000000 ) ) ;
#9432 = CARTESIAN_POINT ( 'NONE',  ( 5.299999999999999822, 0.000000000000000000, 0.000000000000000000 ) ) ;
#9433 = AXIS2_PLACEMENT_3D ( 'NONE', #13208, #8427, #16671 ) ;
#9434 = CARTESIAN_POINT ( 'NONE',  ( -35.09675569278795138, 377.2448905683720000, 15.47720386886985366 ) ) ;
#9435 = CARTESIAN_POINT ( 'NONE',  ( -14.48388495494901740, 499.8073905683720568, -9.489475012073736337 ) ) ;
#9436 = AXIS2_PLACEMENT_3D ( 'NONE', #16522, #9793, #16415 ) ;
#9437 = CARTESIAN_POINT ( 'NONE',  ( -48.68588794268872277, 496.9323905601784759, -3.978247347593158345 ) ) ;
#9438 = CARTESIAN_POINT ( 'NONE',  ( -11.93348319268871727, 319.1823905683720568, -3.332260488124732856 ) ) ;
#9439 = EDGE_CURVE ( 'NONE', #10338, #2613, #17725, .T. ) ;
#9440 = ORIENTED_EDGE ( 'NONE', *, *, #20677, .F. ) ;
#9441 = CARTESIAN_POINT ( 'NONE',  ( 0.2578475836320677783, 4.367703157927326885, -5.434916218090831030 ) ) ;
#9442 = ORIENTED_EDGE ( 'NONE', *, *, #15987, .F. ) ;
#9443 =( BOUNDED_CURVE ( )  B_SPLINE_CURVE ( 2, ( #1950, #10146, #6894, #11982, #539, #8733, #15358, #7106, #13726, #20316, #18147, #16544, #1729, #1319, #17145, #5556, #9519 ),
 .UNSPECIFIED., .F., .T. ) 
 B_SPLINE_CURVE_WITH_KNOTS ( ( 3, 2, 2, 2, 2, 2, 2, 2, 3 ),
 ( 0.3437500000000001110, 0.3457031250000001110, 0.3476562500000001110, 0.3496093750000001110, 0.3515625000000001110, 0.3535156250000001110, 0.3554687500000001110, 0.3574218750000001110, 0.3593750000000001110 ),
 .UNSPECIFIED. ) 
 CURVE ( )  GEOMETRIC_REPRESENTATION_ITEM ( )  RATIONAL_B_SPLINE_CURVE ( ( 0.9999999999999988898, 0.9807852804032315408, 1.000000000000000000, 0.9807852804032304306, 1.000000000000000000, 0.9807852804032304306, 1.000000000000000000, 0.9807852804032304306, 1.000000000000000000, 0.9807852804032304306, 1.000000000000000000, 0.9807852804032304306, 1.000000000000000000, 0.9807852804032304306, 1.000000000000000000, 0.9807852804032293204, 1.000000000000001110 ) ) 
 REPRESENTATION_ITEM ( '' )  );
#9444 = CARTESIAN_POINT ( 'NONE',  ( -49.57497958038186425, 230.5765313837437418, -60.00000000000000000 ) ) ;
#9445 = CARTESIAN_POINT ( 'NONE',  ( -45.43829269268871940, 415.6823905683720568, 3.332260488124734632 ) ) ;
#9446 = FACE_OUTER_BOUND ( 'NONE', #1945, .T. ) ;
#9447 = CARTESIAN_POINT ( 'NONE',  ( -35.09675569278795848, 451.9948905683720000, -15.47720386886985544 ) ) ;
#9448 = ORIENTED_EDGE ( 'NONE', *, *, #20524, .T. ) ;
#9449 = CARTESIAN_POINT ( 'NONE',  ( -16.84014894278199748, 457.6198905683720568, 11.84573899990672530 ) ) ;
#9450 = CARTESIAN_POINT ( 'NONE',  ( 0.000000000000000000, 0.000000000000000000, 0.000000000000000000 ) ) ;
#9451 = CARTESIAN_POINT ( 'NONE',  ( -24.70764059509556532, 414.4323905601784759, -19.99999999999999289 ) ) ;
#9452 = EDGE_CURVE ( 'NONE', #2936, #12320, #21221, .T. ) ;
#9453 = CIRCLE ( 'NONE', #17742, 4.000000000000000000 ) ;
#9454 = CARTESIAN_POINT ( 'NONE',  ( -48.68588794268870856, 382.3073905765656377, 3.978247347593168115 ) ) ;
#9455 = CARTESIAN_POINT ( 'NONE',  ( -48.68588794268860909, 281.6823905765656377, -3.978247347593371508 ) ) ;
#9456 = DIRECTION ( 'NONE',  ( -1.191790137725560488E-16, 1.000000000000000000, -0.000000000000000000 ) ) ;
#9457 = LINE ( 'NONE', #9130, #14990 ) ;
#9458 = CARTESIAN_POINT ( 'NONE',  ( 0.000000000000000000, 0.000000000000000000, -6.499999999999999112 ) ) ;
#9459 = AXIS2_PLACEMENT_3D ( 'NONE', #9267, #20632, #12199 ) ;
#9460 = DIRECTION ( 'NONE',  ( 0.000000000000000000, 0.000000000000000000, 1.000000000000000000 ) ) ;
#9461 = CARTESIAN_POINT ( 'NONE',  ( -11.73070664223723547, 253.1823905601785043, -11.32908994701042538 ) ) ;
#9462 = CARTESIAN_POINT ( 'NONE',  ( 154.7587007620219026, 610.7448905601785327, 10.81142786866622885 ) ) ;
#9463 = CARTESIAN_POINT ( 'NONE',  ( -16.84014894278199748, 431.6198905683720000, -11.84573899990672707 ) ) ;
#9464 = DIRECTION ( 'NONE',  ( 0.5877852522924732481, 7.005166667826999217E-17, 0.8090169943749473402 ) ) ;
#9465 = CARTESIAN_POINT ( 'NONE',  ( -28.68588794268870146, 242.8698905683720568, -16.75240474999999307 ) ) ;
#9466 = ORIENTED_EDGE ( 'NONE', *, *, #16976, .T. ) ;
#9467 = ORIENTED_EDGE ( 'NONE', *, *, #4958, .T. ) ;
#9468 = DIRECTION ( 'NONE',  ( 0.000000000000000000, -1.000000000000000000, 0.000000000000000000 ) ) ;
#9469 = EDGE_LOOP ( 'NONE', ( #16059, #14779, #9087 ) ) ;
#9470 = CARTESIAN_POINT ( 'NONE',  ( -42.88789093042844769, 456.3073905683720000, 9.489475012073734561 ) ) ;
#9471 = CARTESIAN_POINT ( 'NONE',  ( -24.70764059509554045, 219.1823905765656377, -19.99999999999999289 ) ) ;
#9472 = VECTOR ( 'NONE', #7042, 1000.000000000000000 ) ;
#9473 = ORIENTED_EDGE ( 'NONE', *, *, #6048, .F. ) ;
#9474 = FACE_OUTER_BOUND ( 'NONE', #9886, .T. ) ;
#9475 = CARTESIAN_POINT ( 'NONE',  ( -14.48388495494898365, 229.8073905683720000, -9.489475012073736337 ) ) ;
#9476 = ORIENTED_EDGE ( 'NONE', *, *, #717, .F. ) ;
#9477 = CARTESIAN_POINT ( 'NONE',  ( -35.09675569278796559, 531.9948905683720568, -15.47720386886985544 ) ) ;
#9478 = DIRECTION ( 'NONE',  ( 1.776356839400250465E-15, 0.000000000000000000, 1.000000000000000000 ) ) ;
#9479 = CARTESIAN_POINT ( 'NONE',  ( -32.66413529028188378, 439.8073905765656946, -19.99999999999999289 ) ) ;
#9480 = CARTESIAN_POINT ( 'NONE',  ( 0.5805565836007611225, -3.752776749732563033, 6.500000000000000000 ) ) ;
#9481 = DIRECTION ( 'NONE',  ( 1.000000000000000000, 0.000000000000000000, 0.000000000000000000 ) ) ;
#9482 = CARTESIAN_POINT ( 'NONE',  ( -32.66413529028185536, 239.8073905765656377, -19.99999999999999289 ) ) ;
#9483 = ADVANCED_FACE ( 'NONE', ( #3050 ), #21111, .T. ) ;
#9484 = CARTESIAN_POINT ( 'NONE',  ( -14.54375231895775755, 290.9948905601784759, 14.14213562373094568 ) ) ;
#9485 = EDGE_CURVE ( 'NONE', #10233, #16560, #6490, .T. ) ;
#9486 = CARTESIAN_POINT ( 'NONE',  ( -8.685887942688713892, 223.9102039777116886, 2.449293598294704541E-15 ) ) ;
#9487 = CARTESIAN_POINT ( 'NONE',  ( -32.01814843081343298, 221.6823905683720000, -16.75240474999999307 ) ) ;
#9488 = CARTESIAN_POINT ( 'NONE',  ( -14.48388495494899431, 321.3073905683720000, -9.489475012073736337 ) ) ;
#9489 = CARTESIAN_POINT ( 'NONE',  ( -13.68588794268873698, 548.2448905601784190, 0.000000000000000000 ) ) ;
#9490 = CARTESIAN_POINT ( 'NONE',  ( -45.64106924314017988, 378.1823905601785327, 11.32908994701042538 ) ) ;
#9491 = CARTESIAN_POINT ( 'NONE',  ( -25.35362745456397349, 308.1823905683719431, 16.75240474999998952 ) ) ;
#9492 = CARTESIAN_POINT ( 'NONE',  ( -16.84014894278199037, 387.6198905683720568, 11.84573899990672530 ) ) ;
#9493 = CARTESIAN_POINT ( 'NONE',  ( -13.20868407381887977, 520.9948905683720568, -6.410867750099233042 ) ) ;
#9494 = CARTESIAN_POINT ( 'NONE',  ( -21.03221929538690915, 360.3698905601784759, 18.47759065022572500 ) ) ;
#9495 = CARTESIAN_POINT ( 'NONE',  ( -42.82802356641966668, 405.9948905601785327, -14.14213562373094746 ) ) ;
#9496 = ORIENTED_EDGE ( 'NONE', *, *, #4719, .F. ) ;
#9497 = CARTESIAN_POINT ( 'NONE',  ( -35.09675569278795848, 483.4948905683720000, -15.47720386886985544 ) ) ;
#9498 = CARTESIAN_POINT ( 'NONE',  ( -22.30770786884145451, 56.85652257517428865, -152.3753892284480003 ) ) ;
#9499 = CARTESIAN_POINT ( 'NONE',  ( -32.01814843081344009, 286.0573905683720568, 16.75240474999999307 ) ) ;
#9500 = ORIENTED_EDGE ( 'NONE', *, *, #2238, .F. ) ;
#9501 = CARTESIAN_POINT ( 'NONE',  ( -13.20868407381885135, 290.9948905683720000, -6.410867750099233042 ) ) ;
#9502 = CARTESIAN_POINT ( 'NONE',  ( -32.01814843081344719, 331.6823905683720000, -16.75240474999999307 ) ) ;
#9503 = CARTESIAN_POINT ( 'NONE',  ( -8.685887942688710339, 256.6823905765656377, 3.978247347593161010 ) ) ;
#9504 = CARTESIAN_POINT ( 'NONE',  ( -8.685887942688726326, 392.2448905601784759, -2.449293598294705724E-15 ) ) ;
#9505 = CARTESIAN_POINT ( 'NONE',  ( -25.35362745456396283, 226.6823905683720284, 16.75240474999998952 ) ) ;
#9506 = CARTESIAN_POINT ( 'NONE',  ( -14.48388495494899963, 379.4323905683721136, 9.489475012073732785 ) ) ;
#9507 = CARTESIAN_POINT ( 'NONE',  ( -42.99819559747531628, 202.9232509211816478, 4.491669896562675568 ) ) ;
#9508 = CARTESIAN_POINT ( 'NONE',  ( -8.685887942688736985, 492.2448905601785327, -2.449293598294705724E-15 ) ) ;
#9509 = CARTESIAN_POINT ( 'NONE',  ( -36.33955658999052929, 510.1198905765655809, -18.47759065022572855 ) ) ;
#9510 = CARTESIAN_POINT ( 'NONE',  ( -25.35362745456400191, 451.0573905683719431, -16.75240474999999307 ) ) ;
#9511 = DIRECTION ( 'NONE',  ( 0.9510565162951535312, 1.133459776540192417E-16, -0.3090169943749475068 ) ) ;
#9512 = ORIENTED_EDGE ( 'NONE', *, *, #20586, .T. ) ;
#9513 = CARTESIAN_POINT ( 'NONE',  ( -14.54375231895777532, 430.9948905601784759, 14.14213562373094568 ) ) ;
#9514 = ORIENTED_EDGE ( 'NONE', *, *, #20422, .T. ) ;
#9515 = ORIENTED_EDGE ( 'NONE', *, *, #9407, .T. ) ;
#9516 = VERTEX_POINT ( 'NONE', #4878 ) ;
#9517 = CARTESIAN_POINT ( 'NONE',  ( -47.16347859291444422, 352.6198905765656377, 7.653668647301805628 ) ) ;
#9518 = CARTESIAN_POINT ( 'NONE',  ( -24.70764059509554755, 320.0573905601784759, 19.99999999999998934 ) ) ;
#9519 = CARTESIAN_POINT ( 'NONE',  ( -8.685887942688728103, 416.9948905765656377, -2.449293598294705724E-15 ) ) ;
#9520 = CARTESIAN_POINT ( 'NONE',  ( -45.43829269268871229, 345.3698905683720568, 0.000000000000000000 ) ) ;
#9521 = CYLINDRICAL_SURFACE ( 'NONE', #1433, 19.99999999999999645 ) ;
#9522 = CARTESIAN_POINT ( 'NONE',  ( -24.70764059509556887, 504.8073905765656377, 19.99999999999998934 ) ) ;
#9523 = CARTESIAN_POINT ( 'NONE',  ( -19.19641293061498999, 390.4323905683720568, -14.20200298773971603 ) ) ;
#9524 = CARTESIAN_POINT ( 'NONE',  ( -42.88789093042841927, 224.4323905683720000, -9.489475012073736337 ) ) ;
#9525 = CARTESIAN_POINT ( 'NONE',  ( -19.19641293061498644, 390.4323905683721136, -14.20200298773971603 ) ) ;
#9526 = CARTESIAN_POINT ( 'NONE',  ( -10.20829729246298179, 327.6198905765656377, -7.653668647301794969 ) ) ;
#9527 = CARTESIAN_POINT ( 'NONE',  ( -32.66413529028187668, 425.0573905601784759, -19.99999999999999289 ) ) ;
#9528 = CARTESIAN_POINT ( 'NONE',  ( -16.84014894278197971, 287.6198905683720000, 11.84573899990672530 ) ) ;
#9529 =( NAMED_UNIT ( * ) SI_UNIT ( $, .STERADIAN. ) SOLID_ANGLE_UNIT ( ) );
#9530 = CARTESIAN_POINT ( 'NONE',  ( -11.93348319268872970, 440.6823905683721136, -3.332260488124732856 ) ) ;
#9531 = CARTESIAN_POINT ( 'NONE',  ( -28.68588794268870501, 284.7448905601784759, -19.99999999999999289 ) ) ;
#9532 = CARTESIAN_POINT ( 'NONE',  ( -24.70764059509554755, 370.0573905601783622, 19.99999999999998934 ) ) ;
#9533 = LINE ( 'NONE', #10942, #9186 ) ;
#9534 = CARTESIAN_POINT ( 'NONE',  ( -28.68588794268871212, 347.8698905683720568, 16.75240474999999307 ) ) ;
#9535 = CARTESIAN_POINT ( 'NONE',  ( -28.68588794268872988, 496.3698905683720568, 16.75240474999999307 ) ) ;
#9536 = CARTESIAN_POINT ( 'NONE',  ( -24.70764059509557953, 514.4323905601785327, -19.99999999999999289 ) ) ;
#9537 = CARTESIAN_POINT ( 'NONE',  ( -40.53162694259543741, 332.6198905683720000, -11.84573899990672707 ) ) ;
#9538 = EDGE_CURVE ( 'NONE', #18164, #10102, #11473, .T. ) ;
#9539 = VECTOR ( 'NONE', #9003, 1000.000000000000000 ) ;
#9540 = ORIENTED_EDGE ( 'NONE', *, *, #11811, .F. ) ;
#9541 = CARTESIAN_POINT ( 'NONE',  ( 60.03793209889851568, 30.52886280891152282, -131.1729372809869005 ) ) ;
#9542 = ORIENTED_EDGE ( 'NONE', *, *, #7052, .F. ) ;
#9543 = LINE ( 'NONE', #1448, #8434 ) ;
#9544 = CARTESIAN_POINT ( 'NONE',  ( 166.1493775951145437, 620.7448905601785327, 8.917803138848105604 ) ) ;
#9545 = VECTOR ( 'NONE', #1492, 1000.000000000000000 ) ;
#9546 = CARTESIAN_POINT ( 'NONE',  ( -44.16309181155857289, 415.9948905683720000, 6.410867750099241924 ) ) ;
#9547 = CYLINDRICAL_SURFACE ( 'NONE', #15931, 5.000000000000001776 ) ;
#9548 = CARTESIAN_POINT ( 'NONE',  ( -42.88789093042844058, 434.8073905683720568, 9.489475012073736337 ) ) ;
#9549 = VERTEX_POINT ( 'NONE', #12897 ) ;
#9550 = CARTESIAN_POINT ( 'NONE',  ( -19.19641293061499709, 470.4323905683719431, -14.20200298773971603 ) ) ;
#9551 = DIRECTION ( 'NONE',  ( 0.000000000000000000, 0.000000000000000000, 1.000000000000000000 ) ) ;
#9552 = FACE_OUTER_BOUND ( 'NONE', #8181, .T. ) ;
#9553 = CARTESIAN_POINT ( 'NONE',  ( -32.66413529028187668, 384.1823905765655809, 19.99999999999999289 ) ) ;
#9554 = CARTESIAN_POINT ( 'NONE',  ( -11.05500197003667751, 54.24389605313263019, 46.36189423322173297 ) ) ;
#9555 = DIRECTION ( 'NONE',  ( 0.000000000000000000, 1.000000000000000000, -0.000000000000000000 ) ) ;
#9556 = DIRECTION ( 'NONE',  ( 0.000000000000000000, 0.000000000000000000, -1.000000000000000000 ) ) ;
#9557 = CARTESIAN_POINT ( 'NONE',  ( -11.73070664223723369, 256.0573905765656377, 11.32908994701042005 ) ) ;
#9558 = ADVANCED_FACE ( 'NONE', ( #16465 ), #4768, .T. ) ;
#9559 = CIRCLE ( 'NONE', #20269, 49.60091809715359545 ) ;
#9560 = DIRECTION ( 'NONE',  ( 0.000000000000000000, 0.000000000000000000, -1.000000000000000000 ) ) ;
#9561 = DIRECTION ( 'NONE',  ( 0.000000000000000000, 0.000000000000000000, -1.000000000000000000 ) ) ;
#9562 = CARTESIAN_POINT ( 'NONE',  ( -8.685887942688543362, 342.5573905601784190, -3.978247347592740013 ) ) ;
#9563 = VECTOR ( 'NONE', #16546, 1000.000000000000000 ) ;
#9564 = CARTESIAN_POINT ( 'NONE',  ( -44.16309181155857289, 425.9948905683720568, 6.410867750099241924 ) ) ;
#9565 = PLANE ( 'NONE',  #7825 ) ;
#9566 =( BOUNDED_CURVE ( )  B_SPLINE_CURVE ( 2, ( #5439, #12153, #15625, #18630, #812, #8897, #2107, #10410, #594, #17137, #12039 ),
 .UNSPECIFIED., .F., .T. ) 
 B_SPLINE_CURVE_WITH_KNOTS ( ( 3, 2, 2, 2, 2, 3 ),
 ( 0.9531250000000001110, 0.9550781250000001110, 0.9570312500000001110, 0.9589843750000000000, 0.9609375000000000000, 0.9627616638092109103 ),
 .UNSPECIFIED. ) 
 CURVE ( )  GEOMETRIC_REPRESENTATION_ITEM ( )  RATIONAL_B_SPLINE_CURVE ( ( 0.9999999999999988898, 0.9807852804032315408, 1.000000000000000000, 0.9807852804032304306, 1.000000000000000000, 0.9807852804032304306, 1.000000000000000000, 0.9807852804032304306, 1.000000000000000000, 0.9820539924006078669, 0.9976301173658341792 ) ) 
 REPRESENTATION_ITEM ( '' )  );
#9567 = CARTESIAN_POINT ( 'NONE',  ( -22.27502019258947286, 252.2448905683720284, -15.47720386886985544 ) ) ;
#9568 = EDGE_CURVE ( 'NONE', #12017, #5497, #9841, .T. ) ;
#9569 = EDGE_LOOP ( 'NONE', ( #14836, #17561, #8979, #19111 ) ) ;
#9570 = DIRECTION ( 'NONE',  ( 1.000000000000000000, 0.000000000000000000, 3.836511174089486666E-16 ) ) ;
#9571 = ORIENTED_EDGE ( 'NONE', *, *, #12310, .F. ) ;
#9572 = CARTESIAN_POINT ( 'NONE',  ( -32.01814843081345430, 463.1823905683720000, -16.75240474999999307 ) ) ;
#9573 = CARTESIAN_POINT ( 'NONE',  ( -40.01497788969912506, 220.4323905765656093, -16.95518130045146421 ) ) ;
#9574 = CIRCLE ( 'NONE', #12344, 4.000000000000001776 ) ;
#9575 = VERTEX_POINT ( 'NONE', #9634 ) ;
#9576 = CARTESIAN_POINT ( 'NONE',  ( -8.938426032941704028E-16, 600.7448905601785327, -7.500000000000000000 ) ) ;
#9577 = CARTESIAN_POINT ( 'NONE',  ( -20.29730442459490547, 220.5357903062123626, -14.50085278415678403 ) ) ;
#9578 = ORIENTED_EDGE ( 'NONE', *, *, #13647, .F. ) ;
#9579 = CARTESIAN_POINT ( 'NONE',  ( -42.88789093042845479, 532.9323905683720568, -9.489475012073734561 ) ) ;
#9580 = CARTESIAN_POINT ( 'NONE',  ( 91.21585410611801592, 56.85652257517428865, 85.46735025547120301 ) ) ;
#9581 = CONICAL_SURFACE ( 'NONE', #1304, 3.309499999999999886, 0.7853981633974432830 ) ;
#9582 = CARTESIAN_POINT ( 'NONE',  ( -36.33955658999052218, 443.8698905765656377, 18.47759065022572500 ) ) ;
#9583 = PRODUCT ( 'Reciprocating Press Ram Head', 'Reciprocating Press Ram Head', '', ( #18416 ) ) ;
#9584 = CARTESIAN_POINT ( 'NONE',  ( 0.5805565836007702263, -7.505553499465148271, -1.692530754021427292E-16 ) ) ;
#9585 = CARTESIAN_POINT ( 'NONE',  ( -14.48388495494899786, 339.8073905683720000, -9.489475012073734561 ) ) ;
#9586 = LINE ( 'NONE', #11212, #17716 ) ;
#9587 = PLANE ( 'NONE',  #1487 ) ;
#9588 = CARTESIAN_POINT ( 'NONE',  ( -40.01497788969912506, 288.8073905601785327, 16.95518130045146776 ) ) ;
#9589 = FACE_OUTER_BOUND ( 'NONE', #14289, .T. ) ;
#9590 = CARTESIAN_POINT ( 'NONE',  ( -42.88789093042841927, 232.9323905683720000, -9.489475012073736337 ) ) ;
#9591 = CARTESIAN_POINT ( 'NONE',  ( -25.35362745456397349, 308.1823905683719431, 16.75240474999998952 ) ) ;
#9592 = DIRECTION ( 'NONE',  ( -0.000000000000000000, 1.000000000000000000, -0.000000000000000000 ) ) ;
#9593 = DIRECTION ( 'NONE',  ( -0.000000000000000000, -0.000000000000000000, 1.000000000000000000 ) ) ;
#9594 = CARTESIAN_POINT ( 'NONE',  ( -14.48388495494899075, 309.4323905683720568, 9.489475012073732785 ) ) ;
#9595 = CARTESIAN_POINT ( 'NONE',  ( -14.48388495494900141, 369.8073905683720000, -9.489475012073736337 ) ) ;
#9596 = CARTESIAN_POINT ( 'NONE',  ( -25.35362745456399836, 518.1823905683720568, 16.75240474999998952 ) ) ;
#9597 = CARTESIAN_POINT ( 'NONE',  ( -8.685887942688724550, 372.2448905601784759, -2.449293598294705724E-15 ) ) ;
#9598 = DIRECTION ( 'NONE',  ( 0.000000000000000000, 0.000000000000000000, 1.000000000000000000 ) ) ;
#9599 = ORIENTED_EDGE ( 'NONE', *, *, #9223, .T. ) ;
#9600 = CARTESIAN_POINT ( 'NONE',  ( -19.19641293061499709, 481.9323905683720000, -14.20200298773971603 ) ) ;
#9601 = DIRECTION ( 'NONE',  ( -1.000000000000000000, 0.000000000000000000, 0.000000000000000000 ) ) ;
#9602 = CARTESIAN_POINT ( 'NONE',  ( -13.20868407381885135, 279.4948905683720000, -6.410867750099233042 ) ) ;
#9603 = ORIENTED_EDGE ( 'NONE', *, *, #10862, .F. ) ;
#9604 = CARTESIAN_POINT ( 'NONE',  ( -25.35362745456396993, 278.1823905683720000, 16.75240474999998952 ) ) ;
#9605 = CARTESIAN_POINT ( 'NONE',  ( -19.19641293061498288, 320.4323905683720568, -14.20200298773971603 ) ) ;
#9606 = CARTESIAN_POINT ( 'NONE',  ( -22.27502019258946220, 258.4948905683720568, 15.47720386886985189 ) ) ;
#9607 = ADVANCED_FACE ( 'NONE', ( #14636 ), #2747, .T. ) ;
#9608 = CARTESIAN_POINT ( 'NONE',  ( -28.68588794268869790, 254.4948905765656093, 19.99999999999999289 ) ) ;
#9609 = CARTESIAN_POINT ( 'NONE',  ( 118.4271928232701043, 31.85652257517428865, 40.00000000000000000 ) ) ;
#9610 = CARTESIAN_POINT ( 'NONE',  ( -32.01814843081343298, 236.0573905683720568, 16.75240474999999307 ) ) ;
#9611 = ADVANCED_FACE ( 'NONE', ( #16573 ), #1758, .T. ) ;
#9612 = CARTESIAN_POINT ( 'NONE',  ( -35.09675569278795138, 377.2448905683720000, 15.47720386886985366 ) ) ;
#9613 = EDGE_CURVE ( 'NONE', #7633, #5562, #12765, .T. ) ;
#9614 = CARTESIAN_POINT ( 'NONE',  ( -42.93756312153262655, 203.3739285472156268, 4.679109617540635924 ) ) ;
#9615 = DIRECTION ( 'NONE',  ( 0.000000000000000000, 0.5000000000000007772, -0.8660254037844381525 ) ) ;
#9616 = CARTESIAN_POINT ( 'NONE',  ( -36.33955658999050087, 270.1198905765655809, -18.47759065022572855 ) ) ;
#9617 = CARTESIAN_POINT ( 'NONE',  ( -16.84014894278199392, 427.6198905683720000, 11.84573899990672530 ) ) ;
#9618 = LINE ( 'NONE', #11136, #4964 ) ;
#9619 = ORIENTED_EDGE ( 'NONE', *, *, #11793, .T. ) ;
#9620 = CARTESIAN_POINT ( 'NONE',  ( -28.68588794268871922, 419.7448905601784759, 19.99999999999999289 ) ) ;
#9621 = EDGE_CURVE ( 'NONE', #6799, #13531, #6918, .T. ) ;
#9622 = ORIENTED_EDGE ( 'NONE', *, *, #10107, .T. ) ;
#9623 = VERTEX_POINT ( 'NONE', #20339 ) ;
#9624 = CARTESIAN_POINT ( 'NONE',  ( -36.33955658999051508, 353.8698905765656377, 18.47759065022572500 ) ) ;
#9625 = CARTESIAN_POINT ( 'NONE',  ( -48.68588794268870146, 307.2448905601784759, 0.000000000000000000 ) ) ;
#9626 = CARTESIAN_POINT ( 'NONE',  ( 5.674999999999999822, 3.752776749732560368, -6.499999999999999112 ) ) ;
#9627 = CARTESIAN_POINT ( 'NONE',  ( -14.48388495494899608, 339.4323905683720000, 9.489475012073731008 ) ) ;
#9628 = CARTESIAN_POINT ( 'NONE',  ( -17.35679799567831338, 508.5573905765655240, -16.95518130045146421 ) ) ;
#9629 = CARTESIAN_POINT ( 'NONE',  ( -35.09675569278795138, 375.7448905683720000, 15.47720386886985366 ) ) ;
#9630 = CARTESIAN_POINT ( 'NONE',  ( -11.93348319268870661, 230.6823905683720284, -3.332260488124732856 ) ) ;
#9631 = CARTESIAN_POINT ( 'NONE',  ( -32.01814843081344719, 386.0573905683720000, 16.75240474999999307 ) ) ;
#9632 = AXIS2_PLACEMENT_3D ( 'NONE', #5674, #10217, #5568 ) ;
#9633 = CARTESIAN_POINT ( 'NONE',  ( -42.82802356641965957, 330.7448905765655809, -14.14213562373094746 ) ) ;
#9634 = CARTESIAN_POINT ( 'NONE',  ( -33.84809828339280102, 56.85652257517428865, 49.33155846391706945 ) ) ;
#9635 = CARTESIAN_POINT ( 'NONE',  ( -40.53162694259543031, 282.6198905683720000, -11.84573899990672707 ) ) ;
#9636 =( NAMED_UNIT ( * ) PLANE_ANGLE_UNIT ( ) SI_UNIT ( $, .RADIAN. ) );
#9637 = CARTESIAN_POINT ( 'NONE',  ( -14.48388495494900852, 441.3073905683720568, -9.489475012073736337 ) ) ;
#9638 = DIRECTION ( 'NONE',  ( -0.000000000000000000, 0.5000000000000011102, 0.8660254037844379305 ) ) ;
#9639 = DIRECTION ( 'NONE',  ( 1.157565925312684532E-16, -0.9253149302858357794, -0.3791995250394160633 ) ) ;
#9640 = AXIS2_PLACEMENT_3D ( 'NONE', #5564, #17048, #7395 ) ;
#9641 = CARTESIAN_POINT ( 'NONE',  ( -48.68588794268872277, 501.9948905765656377, 0.000000000000000000 ) ) ;
#9642 = CARTESIAN_POINT ( 'NONE',  ( -45.43829269268871229, 355.3698905683720568, 0.000000000000000000 ) ) ;
#9643 = CARTESIAN_POINT ( 'NONE',  ( -40.53162694259545873, 505.1198905683720568, 11.84573899990672885 ) ) ;
#9644 = CARTESIAN_POINT ( 'NONE',  ( -11.73070664223726034, 481.3073905601785896, 11.32908994701042005 ) ) ;
#9645 = CARTESIAN_POINT ( 'NONE',  ( -45.43829269268870519, 323.8698905683720000, 0.000000000000000000 ) ) ;
#9646 = AXIS2_PLACEMENT_3D ( 'NONE', #13081, #16227, #19459 ) ;
#9647 = ORIENTED_EDGE ( 'NONE', *, *, #14730, .F. ) ;
#9648 = CARTESIAN_POINT ( 'NONE',  ( -48.68588794268871567, 526.9323905601785327, -3.978247347593212080 ) ) ;
#9649 = VERTEX_POINT ( 'NONE', #13542 ) ;
#9650 = DIRECTION ( 'NONE',  ( 0.000000000000000000, 0.000000000000000000, -1.000000000000000000 ) ) ;
#9651 = CARTESIAN_POINT ( 'NONE',  ( -19.19641293061498644, 401.9323905683720000, -14.20200298773971603 ) ) ;
#9652 = CARTESIAN_POINT ( 'NONE',  ( -45.64106924314016567, 232.9323905765656093, 11.32908994701042538 ) ) ;
#9653 = CARTESIAN_POINT ( 'NONE',  ( -22.30770786884145451, 30.52886280891152282, -122.9933582338429972 ) ) ;
#9654 = CARTESIAN_POINT ( 'NONE',  ( -11.93348319268873148, 448.8698905683720000, -2.051577885510841163E-15 ) ) ;
#9655 = CARTESIAN_POINT ( 'NONE',  ( -11.93348319268873148, 448.5573905683720000, 3.332260488124728859 ) ) ;
#9656 = CARTESIAN_POINT ( 'NONE',  ( 6.416697501590670427, 172.9933428177121471, 69.47976867265059298 ) ) ;
#9657 = CARTESIAN_POINT ( 'NONE',  ( -28.68588794268871567, 384.4948905765656377, 19.99999999999999289 ) ) ;
#9658 = DIRECTION ( 'NONE',  ( -1.000000000000000000, 0.000000000000000000, 0.000000000000000000 ) ) ;
#9659 = CARTESIAN_POINT ( 'NONE',  ( -28.68588794268871922, 389.4948905765656377, -19.99999999999999289 ) ) ;
#9660 = CARTESIAN_POINT ( 'NONE',  ( -1.025382690249029949, 303.6587712403113528, 25.00000000000000000 ) ) ;
#9661 = CARTESIAN_POINT ( 'NONE',  ( 0.000000000000000000, 0.000000000000000000, 6.500000000000000000 ) ) ;
#9662 = CARTESIAN_POINT ( 'NONE',  ( -22.27502019258950128, 492.2448905683720000, -15.47720386886985544 ) ) ;
#9663 = EDGE_CURVE ( 'NONE', #739, #20672, #1049, .T. ) ;
#9664 = CARTESIAN_POINT ( 'NONE',  ( 0.000000000000000000, 326.0737056351150613, 25.00000000000000000 ) ) ;
#9665 = CARTESIAN_POINT ( 'NONE',  ( -21.03221929538690915, 254.1198905601784759, -18.47759065022572855 ) ) ;
#9666 = CARTESIAN_POINT ( 'NONE',  ( -32.66413529028186957, 345.0573905601784759, -19.99999999999999289 ) ) ;
#9667 = CARTESIAN_POINT ( 'NONE',  ( -35.09675569278795138, 413.4948905683720000, -15.47720386886985544 ) ) ;
#9668 = CARTESIAN_POINT ( 'NONE',  ( -32.66413529028186957, 385.0573905601784759, -19.99999999999999289 ) ) ;
#9669 = CIRCLE ( 'NONE', #3809, 15.00000000000000000 ) ;
#9670 = CARTESIAN_POINT ( 'NONE',  ( -19.19641293061496867, 238.8073905683720000, 14.20200298773971426 ) ) ;
#9671 = VERTEX_POINT ( 'NONE', #5403 ) ;
#9672 = ORIENTED_EDGE ( 'NONE', *, *, #3210, .F. ) ;
#9673 = CARTESIAN_POINT ( 'NONE',  ( 60.03793209889851568, 10.52886280891152104, -131.1729372809869005 ) ) ;
#9674 = VERTEX_POINT ( 'NONE', #10058 ) ;
#9675 = CARTESIAN_POINT ( 'NONE',  ( -13.20868407381887266, 460.9948905683720000, -6.410867750099233042 ) ) ;
#9676 = CARTESIAN_POINT ( 'NONE',  ( -11.73070664223723192, 236.0573905765656093, 11.32908994701042005 ) ) ;
#9677 = EDGE_CURVE ( 'NONE', #1192, #19262, #17596, .T. ) ;
#9678 = VERTEX_POINT ( 'NONE', #20023 ) ;
#9679 = CARTESIAN_POINT ( 'NONE',  ( -48.68588794268872988, 521.9948905765656946, 0.000000000000000000 ) ) ;
#9680 = CARTESIAN_POINT ( 'NONE',  ( -16.84014894278200813, 529.1198905683720568, 11.84573899990672530 ) ) ;
#9681 = ORIENTED_EDGE ( 'NONE', *, *, #17363, .F. ) ;
#9682 = CARTESIAN_POINT ( 'NONE',  ( -40.53162694259545873, 505.1198905683720568, 11.84573899990672885 ) ) ;
#9683 = CARTESIAN_POINT ( 'NONE',  ( 51.50493485826542184, 170.1716627696692683, 20.00000000000000355 ) ) ;
#9684 = AXIS2_PLACEMENT_3D ( 'NONE', #20203, #214, #15450 ) ;
#9686 = AXIS2_PLACEMENT_3D ( 'NONE', #1306, #890, #14301 ) ;
#9685 = CARTESIAN_POINT ( 'NONE',  ( -47.16347859291445843, 451.3698905765656377, -7.653668647301793193 ) ) ;
#9687 = CARTESIAN_POINT ( 'NONE',  ( -28.68588794268873698, 548.2448905601784190, 0.000000000000000000 ) ) ;
#9688 = CARTESIAN_POINT ( 'NONE',  ( -28.68588794268870856, 336.3698905683720000, 16.75240474999999307 ) ) ;
#9689 = CARTESIAN_POINT ( 'NONE',  ( -28.68588794268874054, 573.2448905601785327, 0.000000000000000000 ) ) ;
#9690 = CIRCLE ( 'NONE', #16272, 50.00000000000000000 ) ;
#9691 = CARTESIAN_POINT ( 'NONE',  ( 0.000000000000000000, -5.629165124598849879, -3.250000000000003553 ) ) ;
#9692 = CARTESIAN_POINT ( 'NONE',  ( 6.416697501590670427, 217.7548513357008630, -45.00000000000000000 ) ) ;
#9693 = ADVANCED_FACE ( 'NONE', ( #16887 ), #18390, .T. ) ;
#9694 = CARTESIAN_POINT ( 'NONE',  ( -38.17536295476244135, 232.3073905683720568, -14.20200298773971426 ) ) ;
#9695 = CARTESIAN_POINT ( 'NONE',  ( -25.35362745456397704, 318.1823905683720568, 16.75240474999998952 ) ) ;
#9696 = CARTESIAN_POINT ( 'NONE',  ( -48.68588794268865882, 446.9323905601784190, -3.978247347593264927 ) ) ;
#9697 = CARTESIAN_POINT ( 'NONE',  ( -42.82802356641964536, 265.9948905601784759, -14.14213562373094746 ) ) ;
#9698 = CARTESIAN_POINT ( 'NONE',  ( 153.8141120573112630, 628.3356379279406383, 0.000000000000000000 ) ) ;
#9699 = CARTESIAN_POINT ( 'NONE',  ( -32.01814843081344009, 317.5573905683720568, 16.75240474999999307 ) ) ;
#9700 = VECTOR ( 'NONE', #2658, 1000.000000000000000 ) ;
#9701 = PRESENTATION_LAYER_ASSIGNMENT (  '', '', ( #15253 ) ) ;
#9702 = CARTESIAN_POINT ( 'NONE',  ( -40.53162694259545873, 526.6198905683720568, 11.84573899990672885 ) ) ;
#9703 = CARTESIAN_POINT ( 'NONE',  ( -36.33955658999051508, 369.1198905601785327, 18.47759065022572500 ) ) ;
#9704 = ADVANCED_FACE ( 'NONE', ( #1869 ), #5514, .T. ) ;
#9705 = LINE ( 'NONE', #11434, #11865 ) ;
#9706 = ORIENTED_EDGE ( 'NONE', *, *, #1523, .T. ) ;
#9707 = CARTESIAN_POINT ( 'NONE',  ( -19.19641293061499354, 478.8073905683720568, 14.20200298773971426 ) ) ;
#9708 = CARTESIAN_POINT ( 'NONE',  ( -45.43829269268870519, 273.8698905683720000, 0.000000000000000000 ) ) ;
#9709 = AXIS2_PLACEMENT_3D ( 'NONE', #2147, #2677, #1171 ) ;
#9710 = EDGE_LOOP ( 'NONE', ( #18437, #473, #18248, #17350 ) ) ;
#9711 = CARTESIAN_POINT ( 'NONE',  ( -16.84014894278197616, 279.1198905683720568, 11.84573899990672530 ) ) ;
#9712 = CARTESIAN_POINT ( 'NONE',  ( -44.16309181155856578, 313.2448905683720000, -6.410867750099231266 ) ) ;
#9713 = CARTESIAN_POINT ( 'NONE',  ( -16.84014894278197616, 259.1198905683720568, 11.84573899990672530 ) ) ;
#9714 = CARTESIAN_POINT ( 'NONE',  ( -40.01497788969912506, 273.5573905765656377, 16.95518130045146776 ) ) ;
#9715 = CARTESIAN_POINT ( 'NONE',  ( -42.82802356641967378, 475.9948905601784759, -14.14213562373094746 ) ) ;
#9716 = AXIS2_PLACEMENT_3D ( 'NONE', #17952, #3149, #9730 ) ;
#9717 = LINE ( 'NONE', #8085, #18900 ) ;
#9718 = CARTESIAN_POINT ( 'NONE',  ( -42.88789093042843348, 374.4323905683720000, -9.489475012073736337 ) ) ;
#9719 = CARTESIAN_POINT ( 'NONE',  ( 4.700000000000000178, 3.752776749732560368, -6.499999999999999112 ) ) ;
#9720 = CARTESIAN_POINT ( 'NONE',  ( 20.42502041961813575, 262.6374945681020563, 19.33651958906945012 ) ) ;
#9721 = CARTESIAN_POINT ( 'NONE',  ( -13.20868407381886911, 429.4948905683720568, -6.410867750099233042 ) ) ;
#9722 = DIRECTION ( 'NONE',  ( 0.000000000000000000, -0.000000000000000000, 1.000000000000000000 ) ) ;
#9723 = VERTEX_POINT ( 'NONE', #3579 ) ;
#9724 = CARTESIAN_POINT ( 'NONE',  ( -32.66413529028188378, 425.0573905601784759, -19.99999999999999289 ) ) ;
#9725 = ORIENTED_EDGE ( 'NONE', *, *, #9613, .F. ) ;
#9726 = ORIENTED_EDGE ( 'NONE', *, *, #5783, .T. ) ;
#9727 = ORIENTED_EDGE ( 'NONE', *, *, #15379, .F. ) ;
#9728 = DIRECTION ( 'NONE',  ( 0.000000000000000000, 0.000000000000000000, -1.000000000000000000 ) ) ;
#9729 = CARTESIAN_POINT ( 'NONE',  ( -40.01497788969913216, 305.6823905601784190, -16.95518130045146421 ) ) ;
#9730 = DIRECTION ( 'NONE',  ( 1.000000000000000000, 0.000000000000000000, 0.000000000000000000 ) ) ;
#9731 = PRESENTATION_LAYER_ASSIGNMENT (  '', '', ( #8361 ) ) ;
#9732 = CARTESIAN_POINT ( 'NONE',  ( -38.17536295476244845, 336.9323905683720568, 14.20200298773971781 ) ) ;
#9733 = CARTESIAN_POINT ( 'NONE',  ( -32.66413529028189799, 509.8073905765655809, -19.99999999999999289 ) ) ;
#9734 = CARTESIAN_POINT ( 'NONE',  ( -11.93348319268872260, 379.1823905683721136, -3.332260488124732856 ) ) ;
#9735 = DIRECTION ( 'NONE',  ( -1.000000000000000000, -0.000000000000000000, -0.000000000000000000 ) ) ;
#9736 = CARTESIAN_POINT ( 'NONE',  ( -25.35362745456398414, 386.6823905683720000, 16.75240474999998952 ) ) ;
#9737 = CARTESIAN_POINT ( 'NONE',  ( -47.16347859291443712, 322.6198905765655809, 7.653668647301805628 ) ) ;
#9738 = CARTESIAN_POINT ( 'NONE',  ( -28.68588794268872633, 333.8848358243226357, 0.000000000000000000 ) ) ;
#9739 = CARTESIAN_POINT ( 'NONE',  ( -14.48388495494899075, 279.8073905683720000, -9.489475012073734561 ) ) ;
#9740 = DIRECTION ( 'NONE',  ( 0.000000000000000000, 0.5000000000000008882, -0.8660254037844381525 ) ) ;
#9741 = CARTESIAN_POINT ( 'NONE',  ( -35.09675569278795138, 443.4948905683720568, -15.47720386886985544 ) ) ;
#9742 = EDGE_CURVE ( 'NONE', #1881, #11167, #16681, .T. ) ;
#9743 = LINE ( 'NONE', #4670, #10948 ) ;
#9744 = CARTESIAN_POINT ( 'NONE',  ( 0.4053525175235895284, 3.145852061455926663, 6.499999999999999112 ) ) ;
#9745 = FACE_OUTER_BOUND ( 'NONE', #7783, .T. ) ;
#9746 = AXIS2_PLACEMENT_3D ( 'NONE', #12416, #13831, #14272 ) ;
#9747 = CARTESIAN_POINT ( 'NONE',  ( -32.66413529028187668, 449.4323905601785327, 19.99999999999999289 ) ) ;
#9748 = CARTESIAN_POINT ( 'NONE',  ( -42.88789093042843348, 356.3073905683720000, 9.489475012073736337 ) ) ;
#9749 = CARTESIAN_POINT ( 'NONE',  ( -45.43829269268871940, 484.1823905683720000, 3.332260488124734632 ) ) ;
#9750 = ORIENTED_EDGE ( 'NONE', *, *, #481, .F. ) ;
#9751 = CARTESIAN_POINT ( 'NONE',  ( -14.54375231895778420, 483.4948905601784759, -14.14213562373094746 ) ) ;
#9752 = CARTESIAN_POINT ( 'NONE',  ( -19.19641293061497933, 310.4323905683720568, -14.20200298773971603 ) ) ;
#9753 = VERTEX_POINT ( 'NONE', #10168 ) ;
#9754 = CYLINDRICAL_SURFACE ( 'NONE', #13162, 5.000000000000004441 ) ;
#9755 = ORIENTED_EDGE ( 'NONE', *, *, #16425, .F. ) ;
#9756 = CARTESIAN_POINT ( 'NONE',  ( -33.38506921610404277, 53.58597874041705467, 49.37795238679517951 ) ) ;
#9757 = AXIS2_PLACEMENT_3D ( 'NONE', #5462, #11956, #18127 ) ;
#9758 = CARTESIAN_POINT ( 'NONE',  ( -32.01814843081344719, 407.5573905683720568, 16.75240474999999307 ) ) ;
#9759 = CARTESIAN_POINT ( 'NONE',  ( -48.68588794268878672, 232.3073905765656377, 3.978247347592954952 ) ) ;
#9760 = CARTESIAN_POINT ( 'NONE',  ( -19.19641293061498999, 447.3073905683720568, 14.20200298773971426 ) ) ;
#9761 = CARTESIAN_POINT ( 'NONE',  ( -14.48388495494901029, 449.8073905683720000, -9.489475012073734561 ) ) ;
#9762 = CARTESIAN_POINT ( 'NONE',  ( 81.24038404635966515, 30.52886280891152282, -94.99999999999994316 ) ) ;
#9763 = CARTESIAN_POINT ( 'NONE',  ( -47.16347859291445133, 392.6198905765655809, 7.653668647301805628 ) ) ;
#9764 = CARTESIAN_POINT ( 'NONE',  ( -20.71087849649029522, 45.41521113178804114, 48.95842151343376969 ) ) ;
#9765 = CARTESIAN_POINT ( 'NONE',  ( -32.66413529028185536, 265.0573905601784759, -19.99999999999999289 ) ) ;
#9766 = DIRECTION ( 'NONE',  ( 1.000000000000000000, 0.000000000000000000, 0.000000000000000000 ) ) ;
#9767 = CARTESIAN_POINT ( 'NONE',  ( 45.67500000000000426, 4.475777889183788807E-16, -3.309499999999999886 ) ) ;
#9768 = CARTESIAN_POINT ( 'NONE',  ( -11.93348319268873681, 490.3698905683720568, -2.051577885510841163E-15 ) ) ;
#9769 = FACE_OUTER_BOUND ( 'NONE', #120, .T. ) ;
#9770 = CARTESIAN_POINT ( 'NONE',  ( -10.20829729246299777, 462.8698905601785327, -7.653668647301794969 ) ) ;
#9771 = CARTESIAN_POINT ( 'NONE',  ( -47.16347859291446554, 517.8698905601785327, 7.653668647301805628 ) ) ;
#9772 = VECTOR ( 'NONE', #18020, 1000.000000000000000 ) ;
#9773 = CARTESIAN_POINT ( 'NONE',  ( -16.84014894278199748, 411.6198905683720568, -11.84573899990672707 ) ) ;
#9774 = CARTESIAN_POINT ( 'NONE',  ( -8.685887942688605534, 467.3073905765656946, -3.978247347592846594 ) ) ;
#9775 = CARTESIAN_POINT ( 'NONE',  ( -22.27502019258945865, 228.4948905683720284, 15.47720386886985189 ) ) ;
#9776 = ORIENTED_EDGE ( 'NONE', *, *, #17031, .T. ) ;
#9777 = CARTESIAN_POINT ( 'NONE',  ( -28.68588794268874409, 608.2448905601786464, 0.000000000000000000 ) ) ;
#9778 = EDGE_LOOP ( 'NONE', ( #21234, #3254, #105, #14258 ) ) ;
#9779 = CARTESIAN_POINT ( 'NONE',  ( -44.16309181155857289, 445.9948905683720568, 6.410867750099241924 ) ) ;
#9780 = CARTESIAN_POINT ( 'NONE',  ( -45.64106924314017277, 222.9323905765656093, 11.32908994701042715 ) ) ;
#9781 = CIRCLE ( 'NONE', #493, 49.93977357075243617 ) ;
#9782 = VERTEX_POINT ( 'NONE', #16997 ) ;
#9783 = CARTESIAN_POINT ( 'NONE',  ( -45.64106924314020119, 522.9323905765655809, 11.32908994701042538 ) ) ;
#9784 = CARTESIAN_POINT ( 'NONE',  ( -13.20868407381884602, 229.4948905683720284, -6.410867750099233042 ) ) ;
#9785 = AXIS2_PLACEMENT_3D ( 'NONE', #6601, #13222, #19810 ) ;
#9786 = ORIENTED_EDGE ( 'NONE', *, *, #7575, .T. ) ;
#9787 = CARTESIAN_POINT ( 'NONE',  ( -38.17536295476246977, 505.4323905683720568, 14.20200298773971781 ) ) ;
#9788 = CARTESIAN_POINT ( 'NONE',  ( 0.5805565836007647862, 7.505553499465139389, 2.227827669841787811E-16 ) ) ;
#9789 = CARTESIAN_POINT ( 'NONE',  ( -48.68588794268872277, 451.6823905765656377, -3.978247347593158345 ) ) ;
#9790 = CARTESIAN_POINT ( 'NONE',  ( -21.03221929538691626, 298.8698905765656377, -18.47759065022572855 ) ) ;
#9791 = ADVANCED_FACE ( 'NONE', ( #5092 ), #16786, .F. ) ;
#9792 = CARTESIAN_POINT ( 'NONE',  ( -165.7253922195052951, 600.7448905601785327, 108.8355377051282176 ) ) ;
#9793 = DIRECTION ( 'NONE',  ( 1.000000000000000000, 0.000000000000000000, 0.000000000000000000 ) ) ;
#9794 = FACE_OUTER_BOUND ( 'NONE', #14336, .T. ) ;
#9795 = CARTESIAN_POINT ( 'NONE',  ( -24.70764059509554045, 290.0573905601784759, 19.99999999999998934 ) ) ;
#9796 = CARTESIAN_POINT ( 'NONE',  ( -28.68588794268874054, 588.2448905601785327, 0.000000000000000000 ) ) ;
#9797 = DIRECTION ( 'NONE',  ( -1.191790137725560488E-16, 1.000000000000000000, -0.000000000000000000 ) ) ;
#9798 = CARTESIAN_POINT ( 'NONE',  ( -40.53162694259543031, 316.6198905683720568, 11.84573899990672885 ) ) ;
#9799 = CARTESIAN_POINT ( 'NONE',  ( -28.68588794268870146, 269.7448905601784759, 19.99999999999999289 ) ) ;
#9800 = FACE_OUTER_BOUND ( 'NONE', #8693, .T. ) ;
#9801 = AXIS2_PLACEMENT_3D ( 'NONE', #8093, #8203, #14830 ) ;
#9802 = CARTESIAN_POINT ( 'NONE',  ( -38.17536295476244845, 293.8073905683720568, -14.20200298773971426 ) ) ;
#9803 = CARTESIAN_POINT ( 'NONE',  ( -40.53162694259545873, 524.1198905683720568, -11.84573899990672707 ) ) ;
#9804 = CARTESIAN_POINT ( 'NONE',  ( -48.68588794268870856, 357.5573905601784759, 3.978247347593168115 ) ) ;
#9805 = ADVANCED_FACE ( 'NONE', ( #6712 ), #7127, .F. ) ;
#9806 = DIRECTION ( 'NONE',  ( 0.6352526299242171604, 0.000000000000000000, 0.7723044064191046942 ) ) ;
#9807 = VERTEX_POINT ( 'NONE', #6815 ) ;
#9808 = CARTESIAN_POINT ( 'NONE',  ( -42.88789093042844769, 494.4323905683720000, -9.489475012073736337 ) ) ;
#9809 = LINE ( 'NONE', #16432, #13893 ) ;
#9810 = CARTESIAN_POINT ( 'NONE',  ( -22.27502019258947641, 280.7448905683720568, -15.47720386886985544 ) ) ;
#9811 = EDGE_LOOP ( 'NONE', ( #11096, #20731, #233, #2023 ) ) ;
#9812 = CARTESIAN_POINT ( 'NONE',  ( -25.35362745456397349, 288.1823905683720000, 16.75240474999998952 ) ) ;
#9813 = CARTESIAN_POINT ( 'NONE',  ( -19.19641293061497223, 261.9323905683720568, -14.20200298773971603 ) ) ;
#9814 = CARTESIAN_POINT ( 'NONE',  ( -42.82802356641964536, 253.2448905765656377, 14.14213562373094923 ) ) ;
#9815 = DIRECTION ( 'NONE',  ( 0.000000000000000000, -1.000000000000000000, 0.000000000000000000 ) ) ;
#9816 = CARTESIAN_POINT ( 'NONE',  ( -16.84014894278197616, 230.1198905683720000, -11.84573899990672707 ) ) ;
#9817 = CARTESIAN_POINT ( 'NONE',  ( -11.93348319268871194, 269.1823905683720000, -3.332260488124732856 ) ) ;
#9818 = CARTESIAN_POINT ( 'NONE',  ( -42.88789093042843348, 386.3073905683720000, 9.489475012073736337 ) ) ;
#9819 = EDGE_CURVE ( 'NONE', #5108, #10498, #3473, .T. ) ;
#9820 = DIRECTION ( 'NONE',  ( -0.9910178256594274204, -0.1337298367054296500, 0.000000000000000000 ) ) ;
#9821 = CARTESIAN_POINT ( 'NONE',  ( -174.5421710038924061, 585.7448905601785327, -96.70028278950395872 ) ) ;
#9822 = DIRECTION ( 'NONE',  ( 0.000000000000000000, 1.000000000000000000, -0.000000000000000000 ) ) ;
#9823 = CARTESIAN_POINT ( 'NONE',  ( -38.17536295476246266, 422.3073905683720568, -14.20200298773971426 ) ) ;
#9824 = DIRECTION ( 'NONE',  ( 0.000000000000000000, 0.000000000000000000, 1.000000000000000000 ) ) ;
#9825 = VERTEX_POINT ( 'NONE', #8544 ) ;
#9826 = CARTESIAN_POINT ( 'NONE',  ( -32.66413529028188378, 429.4323905601785896, 19.99999999999999289 ) ) ;
#9827 = EDGE_CURVE ( 'NONE', #4925, #21308, #8254, .T. ) ;
#9828 = ORIENTED_EDGE ( 'NONE', *, *, #19394, .T. ) ;
#9829 = CARTESIAN_POINT ( 'NONE',  ( 0.000000000000000000, 0.000000000000000000, -6.499999999999999112 ) ) ;
#9830 = ORIENTED_EDGE ( 'NONE', *, *, #16695, .F. ) ;
#9831 = ORIENTED_EDGE ( 'NONE', *, *, #8952, .F. ) ;
#9832 = CARTESIAN_POINT ( 'NONE',  ( -54.57497958038185715, 160.1716627696692683, 25.00000000000000000 ) ) ;
#9833 = CARTESIAN_POINT ( 'NONE',  ( -21.03221929538691626, 304.1198905601785327, -18.47759065022572855 ) ) ;
#9834 = DIRECTION ( 'NONE',  ( 0.000000000000000000, 0.000000000000000000, 1.000000000000000000 ) ) ;
#9835 = CARTESIAN_POINT ( 'NONE',  ( -45.43829269268871229, 335.0573905683720568, -3.332260488124726638 ) ) ;
#9836 = CARTESIAN_POINT ( 'NONE',  ( -8.685887942688738761, 487.3073905765656377, -3.978247347593165895 ) ) ;
#9837 = CARTESIAN_POINT ( 'NONE',  ( -44.16309181155857289, 373.2448905683720000, -6.410867750099231266 ) ) ;
#9838 = CARTESIAN_POINT ( 'NONE',  ( -21.25395633610896695, 222.1412455016266279, -15.05426537146665389 ) ) ;
#9839 = CARTESIAN_POINT ( 'NONE',  ( -42.88789093042843348, 382.9323905683720000, -9.489475012073734561 ) ) ;
#9840 = CARTESIAN_POINT ( 'NONE',  ( -11.73070664223724613, 307.9323905765656946, -11.32908994701042715 ) ) ;
#9841 = LINE ( 'NONE', #1648, #20357 ) ;
#9842 = CARTESIAN_POINT ( 'NONE',  ( -11.93348319268871194, 288.8698905683720568, -2.051577885510841163E-15 ) ) ;
#9843 = DIRECTION ( 'NONE',  ( 0.000000000000000000, 1.000000000000000000, 0.000000000000000000 ) ) ;
#9844 = CARTESIAN_POINT ( 'NONE',  ( -32.01814843081345430, 437.5573905683720000, 16.75240474999999307 ) ) ;
#9845 = CARTESIAN_POINT ( 'NONE',  ( -33.22918226429612076, 53.10839921601173330, 120.5024273052909081 ) ) ;
#9846 = CARTESIAN_POINT ( 'NONE',  ( 69.79185940953689737, 142.2976266388001250, 40.00000000000000000 ) ) ;
#9847 = CARTESIAN_POINT ( 'NONE',  ( 0.4053525175236805667, 3.145852061456244630, -6.500000000000000000 ) ) ;
#9848 = CARTESIAN_POINT ( 'NONE',  ( -45.43829269268873361, 535.3698905683720568, 0.000000000000000000 ) ) ;
#9849 = CARTESIAN_POINT ( 'NONE',  ( -11.93348319268871904, 350.3698905683720568, -2.051577885510841163E-15 ) ) ;
#9850 = CARTESIAN_POINT ( 'NONE',  ( -14.48388495494901385, 487.9323905683719431, 9.489475012073732785 ) ) ;
#9851 = ORIENTED_EDGE ( 'NONE', *, *, #6160, .F. ) ;
#9852 = CARTESIAN_POINT ( 'NONE',  ( -42.82802356641967378, 488.4948905601784759, 14.14213562373094923 ) ) ;
#9853 = CARTESIAN_POINT ( 'NONE',  ( -42.88789093042842637, 294.8073905683720000, 9.489475012073736337 ) ) ;
#9854 = ORIENTED_EDGE ( 'NONE', *, *, #19661, .T. ) ;
#9855 = CARTESIAN_POINT ( 'NONE',  ( -8.685887942688809815, 346.6823905765656377, 3.978247347593374172 ) ) ;
#9856 = ORIENTED_EDGE ( 'NONE', *, *, #8756, .F. ) ;
#9857 = CYLINDRICAL_SURFACE ( 'NONE', #2230, 21.20245194746112105 ) ;
#9858 = EDGE_CURVE ( 'NONE', #17432, #454, #8761, .T. ) ;
#9859 = ADVANCED_FACE ( 'NONE', ( #17102 ), #8329, .T. ) ;
#9860 = CARTESIAN_POINT ( 'NONE',  ( -32.01814843081344719, 397.5573905683720568, 16.75240474999999307 ) ) ;
#9861 = CARTESIAN_POINT ( 'NONE',  ( -22.62331590640576451, 326.0737056351150613, -11.80838889663595914 ) ) ;
#9862 = DIRECTION ( 'NONE',  ( 0.000000000000000000, 0.000000000000000000, 1.000000000000000000 ) ) ;
#9863 = CARTESIAN_POINT ( 'NONE',  ( -44.16309181155857999, 433.2448905683720000, -6.410867750099231266 ) ) ;
#9864 = CARTESIAN_POINT ( 'NONE',  ( -35.09675569278795138, 441.9948905683720568, -15.47720386886985544 ) ) ;
#9865 = SHAPE_DEFINITION_REPRESENTATION ( #3032, #21199 ) ;
#9866 = DIRECTION ( 'NONE',  ( 1.000000000000000000, 0.000000000000000000, 0.000000000000000000 ) ) ;
#9867 = CARTESIAN_POINT ( 'NONE',  ( -10.20829729246298712, 376.3698905765656377, 7.653668647301790529 ) ) ;
#9868 = DIRECTION ( 'NONE',  ( 0.000000000000000000, 0.000000000000000000, 1.000000000000000000 ) ) ;
#9869 = FACE_OUTER_BOUND ( 'NONE', #18229, .T. ) ;
#9870 = CARTESIAN_POINT ( 'NONE',  ( -48.68588794268862330, 431.6823905765655240, -3.978247347593371508 ) ) ;
#9871 = CARTESIAN_POINT ( 'NONE',  ( -40.01497788969915348, 490.4323905765656377, -16.95518130045146421 ) ) ;
#9872 = CARTESIAN_POINT ( 'NONE',  ( -11.93348319268873858, 500.6823905683720568, -3.332260488124732856 ) ) ;
#9873 = ADVANCED_FACE ( 'NONE', ( #354 ), #2601, .T. ) ;
#9874 = DIRECTION ( 'NONE',  ( -0.4989387216749512355, -0.8666372666885295839, -0.000000000000000000 ) ) ;
#9875 = DIRECTION ( 'NONE',  ( 0.000000000000000000, 1.000000000000000000, 0.000000000000000000 ) ) ;
#9876 = EDGE_CURVE ( 'NONE', #13766, #6118, #15907, .T. ) ;
#9877 =( BOUNDED_CURVE ( )  B_SPLINE_CURVE ( 2, ( #1927, #6977, #6870, #18451, #3636, #10219, #10322, #16842, #2029, #8597, #15332, #13599, #516, #1248, #19199, #2654, #17465 ),
 .UNSPECIFIED., .F., .T. ) 
 B_SPLINE_CURVE_WITH_KNOTS ( ( 3, 2, 2, 2, 2, 2, 2, 2, 3 ),
 ( 0.2812500000000000555, 0.2832031250000000555, 0.2851562500000000555, 0.2871093750000000555, 0.2890625000000001110, 0.2910156250000001110, 0.2929687500000001110, 0.2949218750000001110, 0.2968750000000001110 ),
 .UNSPECIFIED. ) 
 CURVE ( )  GEOMETRIC_REPRESENTATION_ITEM ( )  RATIONAL_B_SPLINE_CURVE ( ( 0.9999999999999994449, 0.9807852804032309857, 1.000000000000000000, 0.9807852804032304306, 1.000000000000000000, 0.9807852804032304306, 1.000000000000000000, 0.9807852804032304306, 1.000000000000000000, 0.9807852804032304306, 1.000000000000000000, 0.9807852804032304306, 1.000000000000000000, 0.9807852804032304306, 1.000000000000000000, 0.9807852804032293204, 1.000000000000001110 ) ) 
 REPRESENTATION_ITEM ( '' )  );
#9878 = EDGE_CURVE ( 'NONE', #18296, #4322, #7448, .T. ) ;
#9879 = VECTOR ( 'NONE', #5098, 1000.000000000000000 ) ;
#9880 = CARTESIAN_POINT ( 'NONE',  ( -38.17536295476245556, 416.9323905683720568, 14.20200298773971781 ) ) ;
#9881 = CARTESIAN_POINT ( 'NONE',  ( -42.82802356641967378, 470.7448905765655809, -14.14213562373094746 ) ) ;
#9882 = CARTESIAN_POINT ( 'NONE',  ( -38.17536295476244135, 223.8073905683720284, -14.20200298773971426 ) ) ;
#9883 = AXIS2_PLACEMENT_3D ( 'NONE', #6770, #8280, #3325 ) ;
#9884 = EDGE_LOOP ( 'NONE', ( #6505, #18999, #1169, #9500 ) ) ;
#9885 = FACE_OUTER_BOUND ( 'NONE', #3091, .T. ) ;
#9886 = EDGE_LOOP ( 'NONE', ( #8986, #8586, #3590, #16348 ) ) ;
#9887 = CARTESIAN_POINT ( 'NONE',  ( -14.48388495494901029, 451.3073905683720568, -9.489475012073734561 ) ) ;
#9888 = CARTESIAN_POINT ( 'NONE',  ( -35.09675569278796559, 531.9948905683720568, -15.47720386886985544 ) ) ;
#9889 = EDGE_CURVE ( 'NONE', #13531, #13961, #10952, .T. ) ;
#9890 = ORIENTED_EDGE ( 'NONE', *, *, #20917, .T. ) ;
#9891 = DIRECTION ( 'NONE',  ( 0.000000000000000000, 0.000000000000000000, -1.000000000000000000 ) ) ;
#9892 = CARTESIAN_POINT ( 'NONE',  ( -16.84014894278197616, 230.1198905683720000, -11.84573899990672707 ) ) ;
#9893 = ORIENTED_EDGE ( 'NONE', *, *, #6691, .F. ) ;
#9894 = CARTESIAN_POINT ( 'NONE',  ( -13.20868407381887621, 508.2448905683720568, 6.410867750099229490 ) ) ;
#9895 = PLANE ( 'NONE',  #17983 ) ;
#9896 = VECTOR ( 'NONE', #19232, 1000.000000000000000 ) ;
#9897 = CARTESIAN_POINT ( 'NONE',  ( -17.35679799567830273, 435.4323905765656377, 16.95518130045146421 ) ) ;
#9898 = DIRECTION ( 'NONE',  ( -1.000000000000000000, -0.000000000000000000, -0.000000000000000000 ) ) ;
#9899 = CARTESIAN_POINT ( 'NONE',  ( -40.01497788969912506, 250.4323905765656377, -16.95518130045146421 ) ) ;
#9900 = CARTESIAN_POINT ( 'NONE',  ( -42.82802356641967378, 453.2448905765656377, 14.14213562373094923 ) ) ;
#9901 = FACE_OUTER_BOUND ( 'NONE', #10791, .T. ) ;
#9902 = CARTESIAN_POINT ( 'NONE',  ( 5.299999999999999822, 0.000000000000000000, 6.500000000000000888 ) ) ;
#9903 = VECTOR ( 'NONE', #11725, 1000.000000000000000 ) ;
#9904 = CARTESIAN_POINT ( 'NONE',  ( 0.05458999538792617262, -1.264741368075143146, -6.499999999999999112 ) ) ;
#9905 = CARTESIAN_POINT ( 'NONE',  ( -11.73070664223726389, 496.0573905765656946, 11.32908994701042005 ) ) ;
#9906 = CARTESIAN_POINT ( 'NONE',  ( -44.16309181155855867, 305.9948905683720568, 6.410867750099241924 ) ) ;
#9907 = CARTESIAN_POINT ( 'NONE',  ( 35.96497763894178945, 230.5765313837437418, 60.00000000000000000 ) ) ;
#9908 = CARTESIAN_POINT ( 'NONE',  ( -36.33955658999050087, 275.3698905601784759, -18.47759065022572855 ) ) ;
#9909 = CARTESIAN_POINT ( 'NONE',  ( -48.68588794268885067, 412.3073905765655809, 3.978247347592849259 ) ) ;
#9910 = CARTESIAN_POINT ( 'NONE',  ( -28.68588794268870856, 292.8698905683720568, -16.75240474999999307 ) ) ;
#9911 = CIRCLE ( 'NONE', #18547, 3.309499999999999886 ) ;
#9912 = CARTESIAN_POINT ( 'NONE',  ( -22.27502019258950128, 502.2448905683720568, -15.47720386886985544 ) ) ;
#9913 = CARTESIAN_POINT ( 'NONE',  ( -17.35679799567829207, 360.6823905601785327, 16.95518130045146421 ) ) ;
#9914 = AXIS2_PLACEMENT_3D ( 'NONE', #9930, #9820, #19355 ) ;
#9915 = DIRECTION ( 'NONE',  ( -0.7723044064191046942, 0.000000000000000000, 0.6352526299242171604 ) ) ;
#9916 = EDGE_LOOP ( 'NONE', ( #7974, #7118, #4806, #10076, #12551, #8727, #19420, #3621, #13271, #13618 ) ) ;
#9917 = CARTESIAN_POINT ( 'NONE',  ( -44.16309181155857999, 475.9948905683720000, 6.410867750099241924 ) ) ;
#9918 = CARTESIAN_POINT ( 'NONE',  ( -28.68588794268874054, 573.2448905601785327, 0.000000000000000000 ) ) ;
#9919 = CARTESIAN_POINT ( 'NONE',  ( -14.48388495494898720, 277.9323905683720000, 9.489475012073732785 ) ) ;
#9920 = EDGE_LOOP ( 'NONE', ( #2895, #7602, #9, #13824 ) ) ;
#9921 = DIRECTION ( 'NONE',  ( 0.000000000000000000, 1.000000000000000000, -0.000000000000000000 ) ) ;
#9922 = CARTESIAN_POINT ( 'NONE',  ( -13.20868407381884957, 289.7448905683720568, 6.410867750099229490 ) ) ;
#9923 = CARTESIAN_POINT ( 'NONE',  ( -32.01814843081343298, 263.1823905683720000, -16.75240474999999307 ) ) ;
#9924 = CARTESIAN_POINT ( 'NONE',  ( -45.64106924314017277, 251.0573905765656093, -11.32908994701042715 ) ) ;
#9925 = CARTESIAN_POINT ( 'NONE',  ( -14.54375231895775045, 230.9948905601784759, 14.14213562373094568 ) ) ;
#9926 = CARTESIAN_POINT ( 'NONE',  ( -17.35679799567828496, 258.5573905765656377, -16.95518130045146421 ) ) ;
#9927 = CARTESIAN_POINT ( 'NONE',  ( -25.35362745456396993, 276.6823905683720000, 16.75240474999998952 ) ) ;
#9928 = CARTESIAN_POINT ( 'NONE',  ( -38.17536295476244845, 386.9323905683721136, 14.20200298773971781 ) ) ;
#9929 = ADVANCED_FACE ( 'NONE', ( #9292 ), #884, .T. ) ;
#9930 = CARTESIAN_POINT ( 'NONE',  ( 78.68120802659203150, 149.7457237375499517, 94.99999999999994316 ) ) ;
#9931 = CARTESIAN_POINT ( 'NONE',  ( -21.03221929538693402, 458.8698905765656377, -18.47759065022572855 ) ) ;
#9932 = CARTESIAN_POINT ( 'NONE',  ( -22.30770786884145451, 30.52886280891152282, -122.9933582338429972 ) ) ;
#9933 = CARTESIAN_POINT ( 'NONE',  ( -13.20868407381886556, 418.2448905683720568, 6.410867750099229490 ) ) ;
#9934 = CARTESIAN_POINT ( 'NONE',  ( -42.82802356641968089, 508.4948905601784759, 14.14213562373094923 ) ) ;
#9935 = ORIENTED_EDGE ( 'NONE', *, *, #12335, .T. ) ;
#9936 = CARTESIAN_POINT ( 'NONE',  ( -11.73070664223725501, 431.3073905601785327, 11.32908994701042005 ) ) ;
#9937 = VERTEX_POINT ( 'NONE', #7557 ) ;
#9938 = CARTESIAN_POINT ( 'NONE',  ( 0.000000000000000000, 135.1716627696692683, 33.59072564020503648 ) ) ;
#9939 = EDGE_LOOP ( 'NONE', ( #9064, #21181, #10575, #2037 ) ) ;
#9940 = ORIENTED_EDGE ( 'NONE', *, *, #5202, .F. ) ;
#9941 = CARTESIAN_POINT ( 'NONE',  ( -45.64106924314017988, 352.9323905765656946, 11.32908994701042538 ) ) ;
#9942 = CARTESIAN_POINT ( 'NONE',  ( -10.20829729246297823, 302.8698905601784759, -7.653668647301794969 ) ) ;
#9943 = LINE ( 'NONE', #4870, #11091 ) ;
#9944 = EDGE_CURVE ( 'NONE', #4208, #6694, #2495, .T. ) ;
#9945 = CARTESIAN_POINT ( 'NONE',  ( -44.16309181155857289, 344.7448905683720568, -6.410867750099231266 ) ) ;
#9946 = ORIENTED_EDGE ( 'NONE', *, *, #3150, .T. ) ;
#9947 = CARTESIAN_POINT ( 'NONE',  ( -48.68588794268872277, 491.6823905765656946, -3.978247347593158345 ) ) ;
#9948 = CARTESIAN_POINT ( 'NONE',  ( -11.93348319268872260, 369.1823905683720000, -3.332260488124732856 ) ) ;
#9949 = CARTESIAN_POINT ( 'NONE',  ( -22.27502019258949062, 380.7448905683720000, -15.47720386886985544 ) ) ;
#9950 = CARTESIAN_POINT ( 'NONE',  ( -10.20829729246297823, 296.3698905765655809, 7.653668647301790529 ) ) ;
#9951 = DIRECTION ( 'NONE',  ( -1.191790137725560488E-16, 1.000000000000000000, -0.000000000000000000 ) ) ;
#9952 = CARTESIAN_POINT ( 'NONE',  ( -28.68588794268870856, 291.3698905683720568, -16.75240474999999307 ) ) ;
#9953 = CARTESIAN_POINT ( 'NONE',  ( -48.68588794268869435, 237.2448905601785043, 0.000000000000000000 ) ) ;
#9954 = CARTESIAN_POINT ( 'NONE',  ( -38.17536295476246266, 443.8073905683720568, -14.20200298773971426 ) ) ;
#9955 = AXIS2_PLACEMENT_3D ( 'NONE', #6126, #16199, #14155 ) ;
#9956 = EDGE_CURVE ( 'NONE', #5552, #7489, #14183, .T. ) ;
#9957 = CARTESIAN_POINT ( 'NONE',  ( -11.73070664223724080, 283.1823905601784759, -11.32908994701042538 ) ) ;
#9958 = EDGE_CURVE ( 'NONE', #14145, #19311, #18919, .T. ) ;
#9959 = CARTESIAN_POINT ( 'NONE',  ( -7.623296525288703052E-18, 0.6351314446054981966, 6.500000000000001776 ) ) ;
#9960 = CARTESIAN_POINT ( 'NONE',  ( -48.68588794268869435, 267.2448905601784759, 0.000000000000000000 ) ) ;
#9961 = CARTESIAN_POINT ( 'NONE',  ( -28.68588794268875120, 610.7448905601785327, 0.000000000000000000 ) ) ;
#9962 = CARTESIAN_POINT ( 'NONE',  ( -44.16309181155856578, 345.9948905683720000, 6.410867750099241924 ) ) ;
#9963 = CARTESIAN_POINT ( 'NONE',  ( -19.19641293061499709, 480.4323905683720568, -14.20200298773971603 ) ) ;
#9964 = ORIENTED_EDGE ( 'NONE', *, *, #1555, .F. ) ;
#9965 = CARTESIAN_POINT ( 'NONE',  ( -17.35679799567830983, 483.8073905601784190, -16.95518130045146421 ) ) ;
#9966 = CARTESIAN_POINT ( 'NONE',  ( -35.09675569278794427, 305.7448905683720568, 15.47720386886985366 ) ) ;
#9967 = VECTOR ( 'NONE', #3397, 1000.000000000000000 ) ;
#9968 = DIRECTION ( 'NONE',  ( 0.000000000000000000, 0.000000000000000000, 1.000000000000000000 ) ) ;
#9969 = ORIENTED_EDGE ( 'NONE', *, *, #1134, .F. ) ;
#9970 = CARTESIAN_POINT ( 'NONE',  ( -32.00363043698316545, 50.57999860063866038, 49.49059492257082127 ) ) ;
#9971 = VECTOR ( 'NONE', #10405, 1000.000000000000000 ) ;
#9972 = CARTESIAN_POINT ( 'NONE',  ( -19.19641293061498644, 408.8073905683720568, 14.20200298773971426 ) ) ;
#9973 = DIRECTION ( 'NONE',  ( 0.000000000000000000, 0.000000000000000000, 1.000000000000000000 ) ) ;
#9974 = CARTESIAN_POINT ( 'NONE',  ( -21.03221929538691271, 385.1198905765656377, 18.47759065022572500 ) ) ;
#9975 = CARTESIAN_POINT ( 'NONE',  ( -13.20868407381886556, 418.2448905683720568, 6.410867750099229490 ) ) ;
#9976 = CARTESIAN_POINT ( 'NONE',  ( -19.19641293061499354, 450.4323905683720000, -14.20200298773971603 ) ) ;
#9977 = APPLICATION_PROTOCOL_DEFINITION ( 'draft international standard', 'automotive_design', 1998, #7485 ) ;
#9978 = LINE ( 'NONE', #166, #12745 ) ;
#9979 = CARTESIAN_POINT ( 'NONE',  ( -32.66413529028187668, 364.1823905765656377, 19.99999999999999289 ) ) ;
#9980 = CARTESIAN_POINT ( 'NONE',  ( -12.15981775011844768, 51.33689851414709437, 46.76771730510184710 ) ) ;
#9981 = CARTESIAN_POINT ( 'NONE',  ( -42.82802356641964536, 265.9948905601784759, -14.14213562373094746 ) ) ;
#9982 = CARTESIAN_POINT ( 'NONE',  ( -17.35679799567831338, 488.5573905765655809, -16.95518130045146421 ) ) ;
#9983 = CARTESIAN_POINT ( 'NONE',  ( -28.68588794268873343, 502.8698905683719431, -16.75240474999999307 ) ) ;
#9984 = FACE_OUTER_BOUND ( 'NONE', #16084, .T. ) ;
#9985 = CARTESIAN_POINT ( 'NONE',  ( -42.99906419454241302, 207.3703986995724335, 4.488953568700488006 ) ) ;
#9986 = CARTESIAN_POINT ( 'NONE',  ( -25.35362745456399836, 412.5573905683719431, -16.75240474999999307 ) ) ;
#9987 = DIRECTION ( 'NONE',  ( 0.000000000000000000, 0.000000000000000000, 1.000000000000000000 ) ) ;
#9988 = CARTESIAN_POINT ( 'NONE',  ( -11.93348319268870839, 240.0573905683720000, 3.332260488124728415 ) ) ;
#9989 = CARTESIAN_POINT ( 'NONE',  ( -11.93348319268872260, 358.5573905683720000, 3.332260488124728415 ) ) ;
#9990 = ORIENTED_EDGE ( 'NONE', *, *, #16431, .T. ) ;
#9991 = CARTESIAN_POINT ( 'NONE',  ( -45.43829269268872650, 533.5573905683720568, -3.332260488124726194 ) ) ;
#9992 = ORIENTED_EDGE ( 'NONE', *, *, #15044, .F. ) ;
#9993 = CARTESIAN_POINT ( 'NONE',  ( -11.93348319268873148, 450.6823905683720568, -3.332260488124732856 ) ) ;
#9994 = CARTESIAN_POINT ( 'NONE',  ( -40.53162694259545873, 532.6198905683720568, -11.84573899990672707 ) ) ;
#9995 = ADVANCED_FACE ( 'NONE', ( #20556 ), #12331, .T. ) ;
#9996 = ORIENTED_EDGE ( 'NONE', *, *, #20302, .F. ) ;
#9997 = CARTESIAN_POINT ( 'NONE',  ( -21.03221929538691626, 430.3698905601784759, 18.47759065022572500 ) ) ;
#9998 = CARTESIAN_POINT ( 'NONE',  ( -28.68588794268872633, 486.3698905683720568, 16.75240474999999307 ) ) ;
#9999 = EDGE_CURVE ( 'NONE', #313, #11409, #1307, .T. ) ;
#10000 = VERTEX_POINT ( 'NONE', #6149 ) ;
#10001 = CARTESIAN_POINT ( 'NONE',  ( -14.48388495494901385, 497.9323905683720568, 9.489475012073731008 ) ) ;
#10002 = CARTESIAN_POINT ( 'NONE',  ( -18.70454317747300976, 45.89000029780063272, -48.58690594643588412 ) ) ;
#10003 = EDGE_CURVE ( 'NONE', #16434, #1235, #4742, .T. ) ;
#10004 = CARTESIAN_POINT ( 'NONE',  ( -45.64106924314019409, 432.9323905765656946, 11.32908994701042715 ) ) ;
#10005 = CARTESIAN_POINT ( 'NONE',  ( -40.01497788969913216, 300.4323905765656377, -16.95518130045146421 ) ) ;
#10006 = CARTESIAN_POINT ( 'NONE',  ( -48.68588794268869435, 251.9948905765656093, 0.000000000000000000 ) ) ;
#10007 = CARTESIAN_POINT ( 'NONE',  ( -21.03221929538691981, 455.1198905765655809, 18.47759065022572500 ) ) ;
#10008 = DIRECTION ( 'NONE',  ( 0.9864615503757148129, 0.000000000000000000, -0.1639927121256943288 ) ) ;
#10009 = CARTESIAN_POINT ( 'NONE',  ( -33.84809828339279392, 55.89938081350750565, 49.33155846391708366 ) ) ;
#10010 =( BOUNDED_CURVE ( )  B_SPLINE_CURVE ( 2, ( #17104, #8864, #13862, #18814, #3995, #2713, #12558, #19153, #4328, #17833, #2603, #9183, #14503, #4542, #7982 ),
 .UNSPECIFIED., .F., .T. ) 
 B_SPLINE_CURVE_WITH_KNOTS ( ( 3, 2, 2, 2, 2, 2, 2, 3 ),
 ( 0.9687500000000001110, 0.9707031250000001110, 0.9726562500000001110, 0.9746093750000000000, 0.9765625000000000000, 0.9785156250000000000, 0.9791718336226143959, 0.9791727248540345041 ),
 .UNSPECIFIED. ) 
 CURVE ( )  GEOMETRIC_REPRESENTATION_ITEM ( )  RATIONAL_B_SPLINE_CURVE ( ( 0.9999999999999988898, 0.9807852804032315408, 1.000000000000000000, 0.9807852804032304306, 1.000000000000000000, 0.9807852804032304306, 1.000000000000000000, 0.9807852804032304306, 1.000000000000000000, 0.9807852804032304306, 1.000000000000000000, 0.9935442612835747589, 0.9914265054520787768, 0.9914265054520787768, 0.9914265054520787768 ) ) 
 REPRESENTATION_ITEM ( '' )  );
#10011 = CARTESIAN_POINT ( 'NONE',  ( 158.8141120573112630, 400.5398297725602674, 0.000000000000000000 ) ) ;
#10012 = CARTESIAN_POINT ( 'NONE',  ( -24.70764059509556532, 494.8073905765656377, 19.99999999999998934 ) ) ;
#10013 = CARTESIAN_POINT ( 'NONE',  ( -11.93348319268871371, 300.3698905683720568, -2.051577885510841163E-15 ) ) ;
#10014 = EDGE_CURVE ( 'NONE', #10551, #17415, #6884, .T. ) ;
#10015 = CARTESIAN_POINT ( 'NONE',  ( -8.685887942688706786, 232.2448905601785043, -2.449293598294705724E-15 ) ) ;
#10016 = CARTESIAN_POINT ( 'NONE',  ( -45.64106924314017277, 266.3073905601784190, -11.32908994701042715 ) ) ;
#10017 = LINE ( 'NONE', #13607, #5069 ) ;
#10018 = CARTESIAN_POINT ( 'NONE',  ( -28.68588794268870146, 287.8698905683720568, 16.75240474999999307 ) ) ;
#10019 = AXIS2_PLACEMENT_3D ( 'NONE', #19719, #4789, #2761 ) ;
#10020 = CARTESIAN_POINT ( 'NONE',  ( -21.03221929538694468, 534.1198905601785327, -18.47759065022572855 ) ) ;
#10021 = CARTESIAN_POINT ( 'NONE',  ( -45.43829269268872650, 505.6823905683720568, 3.332260488124734632 ) ) ;
#10022 = AXIS2_PLACEMENT_3D ( 'NONE', #189, #15109, #6968 ) ;
#10023 = CARTESIAN_POINT ( 'NONE',  ( -8.685887942688616192, 227.3073905765656377, -3.978247347592952732 ) ) ;
#10024 = EDGE_LOOP ( 'NONE', ( #3648, #1661, #9012, #17944 ) ) ;
#10025 = CARTESIAN_POINT ( 'NONE',  ( -45.43829269268871940, 475.6823905683720000, 3.332260488124734632 ) ) ;
#10026 = FACE_OUTER_BOUND ( 'NONE', #8591, .T. ) ;
#10027 = CARTESIAN_POINT ( 'NONE',  ( -13.20868407381884779, 259.4948905683720568, -6.410867750099233042 ) ) ;
#10028 = EDGE_LOOP ( 'NONE', ( #16057, #14683, #1260, #19023, #4440, #16186 ) ) ;
#10029 = FACE_OUTER_BOUND ( 'NONE', #8209, .T. ) ;
#10030 = CARTESIAN_POINT ( 'NONE',  ( -11.93348319268870661, 240.0573905683720000, 3.332260488124728859 ) ) ;
#10031 = CARTESIAN_POINT ( 'NONE',  ( -45.64106924314017277, 242.9323905765656377, 11.32908994701042715 ) ) ;
#10032 = AXIS2_PLACEMENT_3D ( 'NONE', #3706, #3291, #11822 ) ;
#10033 = DIRECTION ( 'NONE',  ( 0.000000000000000000, 0.000000000000000000, -1.000000000000000000 ) ) ;
#10034 = CARTESIAN_POINT ( 'NONE',  ( -10.20829729246297113, 231.6198905601785043, 7.653668647301790529 ) ) ;
#10035 = CARTESIAN_POINT ( 'NONE',  ( 29.72350413846044859, 280.4463447002762564, 20.00000000000000355 ) ) ;
#10036 = CARTESIAN_POINT ( 'NONE',  ( -45.43829269268869808, 263.8698905683720000, 0.000000000000000000 ) ) ;
#10037 = CARTESIAN_POINT ( 'NONE',  ( -28.68588794268871567, 352.8698905683720568, -16.75240474999999307 ) ) ;
#10038 = DIRECTION ( 'NONE',  ( 0.000000000000000000, 0.000000000000000000, 1.000000000000000000 ) ) ;
#10039 = AXIS2_PLACEMENT_3D ( 'NONE', #840, #8922, #10645 ) ;
#10040 = VECTOR ( 'NONE', #16050, 1000.000000000000000 ) ;
#10041 = CARTESIAN_POINT ( 'NONE',  ( -45.43829269268871229, 423.5573905683720000, -3.332260488124726194 ) ) ;
#10042 = CARTESIAN_POINT ( 'NONE',  ( -47.16347859291444422, 341.3698905765655809, -7.653668647301793193 ) ) ;
#10043 = ORIENTED_EDGE ( 'NONE', *, *, #17756, .F. ) ;
#10044 = CARTESIAN_POINT ( 'NONE',  ( -17.35679799567829917, 410.6823905601784759, 16.95518130045146421 ) ) ;
#10045 = ORIENTED_EDGE ( 'NONE', *, *, #19227, .T. ) ;
#10046 = CARTESIAN_POINT ( 'NONE',  ( 292.4526463419396691, 308.2087638784415162, 40.00000000000000000 ) ) ;
#10047 = ORIENTED_EDGE ( 'NONE', *, *, #4843, .T. ) ;
#10048 = EDGE_LOOP ( 'NONE', ( #10307, #12885, #610, #11634 ) ) ;
#10049 = CARTESIAN_POINT ( 'NONE',  ( -25.35362745456401257, 522.5573905683720568, -16.75240474999999307 ) ) ;
#10050 = CARTESIAN_POINT ( 'NONE',  ( -36.33955658999050797, 309.1198905601785327, 18.47759065022572500 ) ) ;
#10051 = DIRECTION ( 'NONE',  ( -0.000000000000000000, -0.000000000000000000, -1.000000000000000000 ) ) ;
#10052 = ADVANCED_FACE ( 'NONE', ( #17625 ), #21192, .T. ) ;
#10053 = CARTESIAN_POINT ( 'NONE',  ( -11.93348319268871727, 330.6823905683721136, -3.332260488124732856 ) ) ;
#10054 = VECTOR ( 'NONE', #5084, 1000.000000000000000 ) ;
#10055 = CARTESIAN_POINT ( 'NONE',  ( -25.35362745456398059, 356.6823905683720568, 16.75240474999998952 ) ) ;
#10056 = CARTESIAN_POINT ( 'NONE',  ( -32.01814843081344719, 361.6823905683721136, -16.75240474999999307 ) ) ;
#10057 = CARTESIAN_POINT ( 'NONE',  ( -42.82802356641965247, 303.2448905765656377, 14.14213562373094923 ) ) ;
#10058 = CARTESIAN_POINT ( 'NONE',  ( 35.96497763894179656, 170.1716627696692683, -57.37501161332323107 ) ) ;
#10059 = EDGE_CURVE ( 'NONE', #17320, #12803, #17831, .T. ) ;
#10060 = CARTESIAN_POINT ( 'NONE',  ( -14.48388495494898720, 267.9323905683720568, 9.489475012073731008 ) ) ;
#10061 = DIRECTION ( 'NONE',  ( 0.000000000000000000, 0.000000000000000000, 1.000000000000000000 ) ) ;
#10062 = CARTESIAN_POINT ( 'NONE',  ( -13.20868407381886556, 419.7448905683720000, 6.410867750099229490 ) ) ;
#10063 = CARTESIAN_POINT ( 'NONE',  ( -28.05669753933457145, 46.82147536802074939, 121.8123201430361888 ) ) ;
#10064 = CARTESIAN_POINT ( 'NONE',  ( -8.685887942688738761, 502.2448905601784190, -2.449293598294705724E-15 ) ) ;
#10065 = CARTESIAN_POINT ( 'NONE',  ( -8.685887942688712116, 276.9948905765656377, -2.449293598294705724E-15 ) ) ;
#10066 = CARTESIAN_POINT ( 'NONE',  ( 2.416697501590669095, 172.9933428177121471, -60.00000000000000000 ) ) ;
#10067 = CARTESIAN_POINT ( 'NONE',  ( -25.35362745456397704, 338.1823905683720000, 16.75240474999998952 ) ) ;
#10068 = CARTESIAN_POINT ( 'NONE',  ( -42.88789093042844769, 484.8073905683720000, 9.489475012073736337 ) ) ;
#10069 = AXIS2_PLACEMENT_3D ( 'NONE', #19554, #19657, #9601 ) ;
#10070 = ORIENTED_EDGE ( 'NONE', *, *, #4843, .F. ) ;
#10071 = AXIS2_PLACEMENT_3D ( 'NONE', #13169, #18129, #16743 ) ;
#10072 = CARTESIAN_POINT ( 'NONE',  ( -21.03221929538692336, 480.3698905601784759, 18.47759065022572500 ) ) ;
#10073 = CARTESIAN_POINT ( 'NONE',  ( -44.16309181155856578, 303.2448905683720000, -6.410867750099231266 ) ) ;
#10074 = EDGE_LOOP ( 'NONE', ( #10658, #18330, #19501, #7330, #1006, #11028 ) ) ;
#10075 = DIRECTION ( 'NONE',  ( 0.4627175328665443232, 0.000000000000000000, -0.8865057725575725689 ) ) ;
#10076 = ORIENTED_EDGE ( 'NONE', *, *, #3454, .T. ) ;
#10077 = DIRECTION ( 'NONE',  ( 1.000000000000000000, 0.000000000000000000, -0.000000000000000000 ) ) ;
#10078 = ADVANCED_FACE ( 'NONE', ( #14608 ), #2817, .T. ) ;
#10079 = CARTESIAN_POINT ( 'NONE',  ( -42.88789093042844058, 404.4323905683721136, -9.489475012073734561 ) ) ;
#10080 = CARTESIAN_POINT ( 'NONE',  ( -17.35679799567829917, 445.4323905765656377, 16.95518130045146421 ) ) ;
#10081 = CARTESIAN_POINT ( 'NONE',  ( -36.33955658999051508, 383.8698905765656377, 18.47759065022572500 ) ) ;
#10082 = CARTESIAN_POINT ( 'NONE',  ( -44.16309181155857289, 424.4948905683720568, 6.410867750099241924 ) ) ;
#10083 = CARTESIAN_POINT ( 'NONE',  ( -25.35362745456396993, 268.1823905683720000, 16.75240474999998952 ) ) ;
#10084 = CARTESIAN_POINT ( 'NONE',  ( -32.01814843081344719, 436.0573905683720568, 16.75240474999999307 ) ) ;
#10085 = APPLICATION_PROTOCOL_DEFINITION ( 'draft international standard', 'automotive_design', 1998, #16890 ) ;
#10086 = DIRECTION ( 'NONE',  ( 0.000000000000000000, 0.000000000000000000, 1.000000000000000000 ) ) ;
#10087 = CARTESIAN_POINT ( 'NONE',  ( -48.68588794268870856, 371.9948905765655809, 0.000000000000000000 ) ) ;
#10088 = DIRECTION ( 'NONE',  ( -0.000000000000000000, -0.000000000000000000, 1.000000000000000000 ) ) ;
#10089 = CARTESIAN_POINT ( 'NONE',  ( -48.68588794268869435, 267.2448905601784759, 0.000000000000000000 ) ) ;
#10090 = CARTESIAN_POINT ( 'NONE',  ( -45.43829269268871229, 333.8698905683720000, 0.000000000000000000 ) ) ;
#10091 = VECTOR ( 'NONE', #14200, 999.9999999999998863 ) ;
#10092 = CARTESIAN_POINT ( 'NONE',  ( -16.84014894278200458, 491.6198905683720000, -11.84573899990672707 ) ) ;
#10093 = CARTESIAN_POINT ( 'NONE',  ( 30.07572094023280940, 170.1716627696692683, 57.31989048965873934 ) ) ;
#10094 = CARTESIAN_POINT ( 'NONE',  ( -6.276925316985663805, 600.7448905601785327, 44.69718552705352010 ) ) ;
#10095 = CARTESIAN_POINT ( 'NONE',  ( -43.63240380007613339, 209.9813597091836641, 1.306460585600322188 ) ) ;
#10096 = EDGE_CURVE ( 'NONE', #5934, #18961, #16927, .T. ) ;
#10097 = CARTESIAN_POINT ( 'NONE',  ( -38.17536295476246266, 403.8073905683721136, -14.20200298773971426 ) ) ;
#10098 = LINE ( 'NONE', #19955, #8160 ) ;
#10099 = VECTOR ( 'NONE', #11074, 1000.000000000000000 ) ;
#10100 = CARTESIAN_POINT ( 'NONE',  ( 8.313338196759850973, 218.8819358349711024, 2.050088646935358305 ) ) ;
#10101 = CARTESIAN_POINT ( 'NONE',  ( -35.09675569278794427, 361.9948905683720568, -15.47720386886985544 ) ) ;
#10102 = VERTEX_POINT ( 'NONE', #6572 ) ;
#10103 = CARTESIAN_POINT ( 'NONE',  ( -38.17536295476247687, 522.3073905683721705, -14.20200298773971426 ) ) ;
#10104 = VERTEX_POINT ( 'NONE', #4540 ) ;
#10105 = CARTESIAN_POINT ( 'NONE',  ( -19.19641293061498999, 448.8073905683721136, 14.20200298773971426 ) ) ;
#10106 = CARTESIAN_POINT ( 'NONE',  ( -19.19641293061499709, 517.3073905683720568, 14.20200298773971426 ) ) ;
#10107 = EDGE_CURVE ( 'NONE', #10687, #2936, #11125, .T. ) ;
#10108 = ORIENTED_EDGE ( 'NONE', *, *, #14790, .T. ) ;
#10109 = CARTESIAN_POINT ( 'NONE',  ( -14.54375231895779130, 528.2448905765656946, -14.14213562373094746 ) ) ;
#10110 = CARTESIAN_POINT ( 'NONE',  ( -38.17536295476246266, 485.4323905683720000, 14.20200298773971781 ) ) ;
#10111 = AXIS2_PLACEMENT_3D ( 'NONE', #16491, #2001, #20049 ) ;
#10112 = ORIENTED_EDGE ( 'NONE', *, *, #6299, .F. ) ;
#10113 = CARTESIAN_POINT ( 'NONE',  ( -11.93348319268873858, 509.1823905683720000, -3.332260488124732856 ) ) ;
#10114 = CARTESIAN_POINT ( 'NONE',  ( -10.76731745429009734, 55.79702461148883685, -46.25122601329427852 ) ) ;
#10115 = CARTESIAN_POINT ( 'NONE',  ( -8.685887942688729879, 427.3073905765655809, -3.978247347593165895 ) ) ;
#10116 = CARTESIAN_POINT ( 'NONE',  ( -28.68588794268871567, 359.4948905765656377, -19.99999999999999289 ) ) ;
#10117 = CARTESIAN_POINT ( 'NONE',  ( -32.66413529028185536, 249.8073905765656662, -19.99999999999999289 ) ) ;
#10118 = LINE ( 'NONE', #16740, #4948 ) ;
#10119 = CARTESIAN_POINT ( 'NONE',  ( -28.68588794268874054, 573.2448905601785327, 0.000000000000000000 ) ) ;
#10120 = CARTESIAN_POINT ( 'NONE',  ( 0.06682554136338426931, -6.264794173742287420, -2.149058192116898081 ) ) ;
#10121 =( GEOMETRIC_REPRESENTATION_CONTEXT ( 3 ) GLOBAL_UNCERTAINTY_ASSIGNED_CONTEXT ( ( #4858 ) ) GLOBAL_UNIT_ASSIGNED_CONTEXT ( ( #4717, #21269, #19641 ) ) REPRESENTATION_CONTEXT ( 'NONE', 'WORKASPACE' ) );
#10122 = FACE_OUTER_BOUND ( 'NONE', #18059, .T. ) ;
#10123 = CARTESIAN_POINT ( 'NONE',  ( -42.99819559747531628, 202.9232509211816478, -4.491669896562675568 ) ) ;
#10124 = CARTESIAN_POINT ( 'NONE',  ( -19.19641293061497933, 301.9323905683720000, -14.20200298773971603 ) ) ;
#10125 = CARTESIAN_POINT ( 'NONE',  ( -14.54375231895778775, 530.9948905601784190, 14.14213562373094568 ) ) ;
#10126 = CARTESIAN_POINT ( 'NONE',  ( -21.03221929538690205, 270.3698905601784759, 18.47759065022572500 ) ) ;
#10127 = DIRECTION ( 'NONE',  ( 1.000000000000000000, 0.000000000000000000, 0.000000000000000000 ) ) ;
#10128 = CARTESIAN_POINT ( 'NONE',  ( -40.53162694259543031, 296.6198905683720000, 11.84573899990672885 ) ) ;
#10129 = CIRCLE ( 'NONE', #10461, 220.7252770684331438 ) ;
#10130 = ORIENTED_EDGE ( 'NONE', *, *, #9217, .T. ) ;
#10131 = CARTESIAN_POINT ( 'NONE',  ( 107.6674317086782935, 187.4856410316723441, 40.00000000000000000 ) ) ;
#10132 = CARTESIAN_POINT ( 'NONE',  ( -28.68588794268872988, 497.8698905683720568, 16.75240474999999307 ) ) ;
#10133 = AXIS2_PLACEMENT_3D ( 'NONE', #14665, #19513, #9556 ) ;
#10134 = ORIENTED_EDGE ( 'NONE', *, *, #7452, .T. ) ;
#10135 = CARTESIAN_POINT ( 'NONE',  ( -42.88789093042844769, 466.3073905683720568, 9.489475012073736337 ) ) ;
#10136 = DIRECTION ( 'NONE',  ( -1.191790137725560488E-16, 1.000000000000000000, -0.000000000000000000 ) ) ;
#10137 = CARTESIAN_POINT ( 'NONE',  ( -44.16309181155855157, 264.4948905683720000, 6.410867750099241924 ) ) ;
#10138 = ADVANCED_FACE ( 'NONE', ( #16019 ), #14399, .F. ) ;
#10139 = VERTEX_POINT ( 'NONE', #4846 ) ;
#10140 =( BOUNDED_CURVE ( )  B_SPLINE_CURVE ( 2, ( #15042, #226, #8842, #18477, #6689, #5179, #11775, #10151, #16767, #1954, #8524, #16871, #15149, #6898, #20111, #10247, #5280 ),
 .UNSPECIFIED., .F., .T. ) 
 B_SPLINE_CURVE_WITH_KNOTS ( ( 3, 2, 2, 2, 2, 2, 2, 2, 3 ),
 ( 0.09375000000000008327, 0.09570312500000012490, 0.09765625000000018041, 0.09960937500000022204, 0.1015625000000002776, 0.1035156250000003192, 0.1054687500000003608, 0.1074218750000004163, 0.1093750000000004580 ),
 .UNSPECIFIED. ) 
 CURVE ( )  GEOMETRIC_REPRESENTATION_ITEM ( )  RATIONAL_B_SPLINE_CURVE ( ( 0.9999999999999992228, 0.9807852804032312077, 1.000000000000000000, 0.9807852804032304306, 1.000000000000000000, 0.9807852804032304306, 1.000000000000000000, 0.9807852804032304306, 1.000000000000000000, 0.9807852804032304306, 1.000000000000000000, 0.9807852804032304306, 1.000000000000000000, 0.9807852804032304306, 1.000000000000000000, 0.9807852804032258787, 1.000000000000004441 ) ) 
 REPRESENTATION_ITEM ( '' )  );
#10141 = DIRECTION ( 'NONE',  ( -1.191790137725560488E-16, 1.000000000000000000, -0.000000000000000000 ) ) ;
#10142 = EDGE_CURVE ( 'NONE', #12371, #368, #3512, .T. ) ;
#10143 = CARTESIAN_POINT ( 'NONE',  ( -19.19641293061496512, 248.8073905683720284, 14.20200298773971426 ) ) ;
#10144 = CIRCLE ( 'NONE', #4959, 4.999999999999990230 ) ;
#10145 = CARTESIAN_POINT ( 'NONE',  ( -10.20829729246297291, 247.6198905765656377, -7.653668647301794969 ) ) ;
#10146 = CARTESIAN_POINT ( 'NONE',  ( -48.68588794268862330, 421.6823905765655240, -3.978247347593371508 ) ) ;
#10147 = CARTESIAN_POINT ( 'NONE',  ( -17.35679799567828496, 233.8073905601784475, -16.95518130045146421 ) ) ;
#10148 = CARTESIAN_POINT ( 'NONE',  ( -38.17536295476244135, 262.3073905683720568, -14.20200298773971426 ) ) ;
#10149 = CIRCLE ( 'NONE', #12586, 6.500000000000000888 ) ;
#10150 = CARTESIAN_POINT ( 'NONE',  ( -28.68588794268871212, 357.8698905683720568, 16.75240474999999307 ) ) ;
#10151 = CARTESIAN_POINT ( 'NONE',  ( -32.66413529028188378, 505.0573905601785327, -19.99999999999999289 ) ) ;
#10152 = CARTESIAN_POINT ( 'NONE',  ( -40.53162694259544452, 412.6198905683720568, -11.84573899990672707 ) ) ;
#10153 = DIRECTION ( 'NONE',  ( 0.000000000000000000, 1.000000000000000000, 0.000000000000000000 ) ) ;
#10154 = ORIENTED_EDGE ( 'NONE', *, *, #12715, .T. ) ;
#10155 = CARTESIAN_POINT ( 'NONE',  ( -42.82802356641966668, 415.9948905601785327, -14.14213562373094746 ) ) ;
#10156 = ORIENTED_EDGE ( 'NONE', *, *, #4472, .F. ) ;
#10157 = VERTEX_POINT ( 'NONE', #19561 ) ;
#10158 = EDGE_LOOP ( 'NONE', ( #17743, #13848, #13399, #15746 ) ) ;
#10159 = CARTESIAN_POINT ( 'NONE',  ( -44.16309181155859420, 534.7448905683720568, -6.410867750099231266 ) ) ;
#10160 = CARTESIAN_POINT ( 'NONE',  ( -28.68588794268870501, 284.7448905601784759, -19.99999999999999289 ) ) ;
#10161 = FACE_OUTER_BOUND ( 'NONE', #19317, .T. ) ;
#10162 = VECTOR ( 'NONE', #20354, 1000.000000000000000 ) ;
#10163 = CARTESIAN_POINT ( 'NONE',  ( -35.09675569278794427, 333.4948905683720568, -15.47720386886985544 ) ) ;
#10164 = ORIENTED_EDGE ( 'NONE', *, *, #16908, .F. ) ;
#10165 = CARTESIAN_POINT ( 'NONE',  ( -35.09675569278795138, 355.7448905683720568, 15.47720386886985366 ) ) ;
#10166 = CARTESIAN_POINT ( 'NONE',  ( -28.68588794268871212, 366.3698905683720568, 16.75240474999999307 ) ) ;
#10167 = CARTESIAN_POINT ( 'NONE',  ( -48.68588794268870146, 311.9948905765655809, 0.000000000000000000 ) ) ;
#10168 = CARTESIAN_POINT ( 'NONE',  ( 81.24038404635966515, 10.52886280891152104, 94.99999999999994316 ) ) ;
#10169 = CARTESIAN_POINT ( 'NONE',  ( -11.93348319268870839, 258.8698905683720000, -2.051577885510841163E-15 ) ) ;
#10170 = CARTESIAN_POINT ( 'NONE',  ( -44.16309181155857999, 424.7448905683720000, -6.410867750099231266 ) ) ;
#10171 = CARTESIAN_POINT ( 'NONE',  ( -8.685887942688712116, 266.9948905765656377, -2.449293598294705724E-15 ) ) ;
#10172 = CARTESIAN_POINT ( 'NONE',  ( -45.43829269268873361, 535.3698905683720568, 0.000000000000000000 ) ) ;
#10173 = CARTESIAN_POINT ( 'NONE',  ( -48.68588794268885067, 407.5573905601785327, 3.978247347592849259 ) ) ;
#10174 = CARTESIAN_POINT ( 'NONE',  ( -19.19641293061497933, 318.8073905683720568, 14.20200298773971426 ) ) ;
#10175 = CARTESIAN_POINT ( 'NONE',  ( -32.01814843081346140, 476.0573905683720000, 16.75240474999999307 ) ) ;
#10176 = VERTEX_POINT ( 'NONE', #12869 ) ;
#10177 = CARTESIAN_POINT ( 'NONE',  ( -17.35679799567830628, 470.6823905601784759, 16.95518130045146421 ) ) ;
#10178 = CARTESIAN_POINT ( 'NONE',  ( -22.27502019258947996, 300.7448905683720568, -15.47720386886985544 ) ) ;
#10179 = CARTESIAN_POINT ( 'NONE',  ( -24.70764059509554755, 344.8073905765656377, 19.99999999999998934 ) ) ;
#10180 = ORIENTED_EDGE ( 'NONE', *, *, #17106, .F. ) ;
#10181 = CARTESIAN_POINT ( 'NONE',  ( 64.58676821086662301, 170.1716627696692683, -57.64290030256307062 ) ) ;
#10182 = CARTESIAN_POINT ( 'NONE',  ( -45.64106924314018698, 348.1823905601784190, 11.32908994701042715 ) ) ;
#10183 = CARTESIAN_POINT ( 'NONE',  ( -38.17536295476246266, 393.8073905683720000, -14.20200298773971426 ) ) ;
#10184 = CARTESIAN_POINT ( 'NONE',  ( 32.47532367400570052, 600.7448905601785327, 163.9643442751439011 ) ) ;
#10185 = DIRECTION ( 'NONE',  ( -1.000000000000000000, 0.000000000000000000, 0.000000000000000000 ) ) ;
#10186 = CARTESIAN_POINT ( 'NONE',  ( -16.84014894278199392, 427.6198905683720000, 11.84573899990672530 ) ) ;
#10187 = CARTESIAN_POINT ( 'NONE',  ( -45.43829269268869098, 255.6823905683720000, 3.332260488124734632 ) ) ;
#10188 = CARTESIAN_POINT ( 'NONE',  ( -28.68588794268872277, 431.3698905683720000, -16.75240474999999307 ) ) ;
#10189 = APPLICATION_PROTOCOL_DEFINITION ( 'draft international standard', 'automotive_design', 1998, #6103 ) ;
#10190 = DIRECTION ( 'NONE',  ( 1.191790137725560488E-16, -1.000000000000000000, -0.000000000000000000 ) ) ;
#10191 = CARTESIAN_POINT ( 'NONE',  ( -8.685887942688722774, 366.6823905765656946, 3.978247347593161010 ) ) ;
#10192 = PLANE ( 'NONE',  #18959 ) ;
#10193 = DIRECTION ( 'NONE',  ( -1.000000000000000000, 0.000000000000000000, 0.000000000000000000 ) ) ;
#10194 = CARTESIAN_POINT ( 'NONE',  ( -38.17536295476245556, 332.3073905683720000, -14.20200298773971426 ) ) ;
#10195 = CARTESIAN_POINT ( 'NONE',  ( -13.68588794268874054, 588.2448905601785327, 0.000000000000000000 ) ) ;
#10196 = CARTESIAN_POINT ( 'NONE',  ( -14.48388495494901385, 471.3073905683720568, -9.489475012073736337 ) ) ;
#10197 = DIRECTION ( 'NONE',  ( -1.854788578061058554E-16, -1.000000000000000000, 0.000000000000000000 ) ) ;
#10198 = CARTESIAN_POINT ( 'NONE',  ( -11.73070664223726212, 463.1823905601784759, -11.32908994701042538 ) ) ;
#10199 = CARTESIAN_POINT ( 'NONE',  ( -40.01497788969913216, 305.6823905601784190, -16.95518130045146421 ) ) ;
#10200 = ADVANCED_FACE ( 'NONE', ( #1510 ), #11234, .F. ) ;
#10201 = CARTESIAN_POINT ( 'NONE',  ( -42.88789093042843348, 384.4323905683720000, -9.489475012073736337 ) ) ;
#10202 = CARTESIAN_POINT ( 'NONE',  ( 162.8695233526006803, 610.7448905601785327, -10.81142786866620575 ) ) ;
#10203 = CARTESIAN_POINT ( 'NONE',  ( -47.16347859291446554, 536.6198905601784190, -7.653668647301793193 ) ) ;
#10204 = CARTESIAN_POINT ( 'NONE',  ( -42.88789093042843348, 372.9323905683720568, -9.489475012073736337 ) ) ;
#10205 = ORIENTED_EDGE ( 'NONE', *, *, #10517, .F. ) ;
#10206 = CARTESIAN_POINT ( 'NONE',  ( -32.01814843081346851, 531.6823905683719431, -16.75240474999999307 ) ) ;
#10207 = ORIENTED_EDGE ( 'NONE', *, *, #14481, .T. ) ;
#10208 = CARTESIAN_POINT ( 'NONE',  ( -35.09675569278797269, 525.7448905683720568, 15.47720386886985366 ) ) ;
#10209 = VERTEX_POINT ( 'NONE', #14714 ) ;
#10210 = CARTESIAN_POINT ( 'NONE',  ( -17.35679799567831694, 528.5573905765656946, -16.95518130045146421 ) ) ;
#10211 = CARTESIAN_POINT ( 'NONE',  ( -16.84014894278200458, 480.1198905683720000, -11.84573899990672707 ) ) ;
#10212 = ORIENTED_EDGE ( 'NONE', *, *, #4215, .T. ) ;
#10213 = CARTESIAN_POINT ( 'NONE',  ( -14.48388495494901029, 487.9323905683719431, 9.489475012073731008 ) ) ;
#10214 = CARTESIAN_POINT ( 'NONE',  ( -12.99034458037978546, 50.04225476994710675, -47.05236843673905867 ) ) ;
#10215 = EDGE_CURVE ( 'NONE', #12217, #1162, #19667, .T. ) ;
#10216 = CARTESIAN_POINT ( 'NONE',  ( -47.16347859291445133, 421.3698905765656377, -7.653668647301793193 ) ) ;
#10217 = DIRECTION ( 'NONE',  ( -0.9510565162951537532, -1.133459776540192910E-16, -0.3090169943749470627 ) ) ;
#10218 = CARTESIAN_POINT ( 'NONE',  ( 158.8141120573112630, 400.5398297725602674, 0.000000000000000000 ) ) ;
#10219 = CARTESIAN_POINT ( 'NONE',  ( -40.01497788969914637, 440.4323905765656946, -16.95518130045146421 ) ) ;
#10220 = CARTESIAN_POINT ( 'NONE',  ( 0.000000000000000000, 0.000000000000000000, 6.500000000000000888 ) ) ;
#10221 = CARTESIAN_POINT ( 'NONE',  ( -45.64106924314018698, 436.3073905601784759, -11.32908994701042538 ) ) ;
#10222 = CARTESIAN_POINT ( 'NONE',  ( -28.68588794268872988, 494.4948905765656377, 19.99999999999999289 ) ) ;
#10223 = CARTESIAN_POINT ( 'NONE',  ( -11.93348319268871549, 300.0573905683720568, 3.332260488124728415 ) ) ;
#10224 = EDGE_CURVE ( 'NONE', #19655, #20672, #5063, .T. ) ;
#10225 = AXIS2_PLACEMENT_3D ( 'NONE', #5100, #16366, #18184 ) ;
#10226 = DIRECTION ( 'NONE',  ( 0.000000000000000000, -0.000000000000000000, 1.000000000000000000 ) ) ;
#10227 = CARTESIAN_POINT ( 'NONE',  ( -16.84014894278200103, 441.6198905683720568, -11.84573899990672707 ) ) ;
#10228 = CARTESIAN_POINT ( 'NONE',  ( -8.685887942688738761, 496.9948905765655809, -2.449293598294705724E-15 ) ) ;
#10229 = CARTESIAN_POINT ( 'NONE',  ( -13.20868407381885135, 290.9948905683720000, -6.410867750099233042 ) ) ;
#10230 = VERTEX_POINT ( 'NONE', #15247 ) ;
#10231 = CARTESIAN_POINT ( 'NONE',  ( -38.17536295476246977, 506.9323905683720000, 14.20200298773971781 ) ) ;
#10232 = AXIS2_PLACEMENT_3D ( 'NONE', #4253, #1024, #12792 ) ;
#10233 = VERTEX_POINT ( 'NONE', #5275 ) ;
#10234 = CARTESIAN_POINT ( 'NONE',  ( -22.27502019258949773, 472.2448905683720568, -15.47720386886985544 ) ) ;
#10235 = CARTESIAN_POINT ( 'NONE',  ( 10.41669750159067220, 172.9933428177121471, 60.00000000000000000 ) ) ;
#10236 = CARTESIAN_POINT ( 'NONE',  ( -44.16309181155855157, 254.4948905683720568, 6.410867750099241924 ) ) ;
#10237 = ORIENTED_EDGE ( 'NONE', *, *, #4464, .T. ) ;
#10238 = PLANE ( 'NONE',  #7973 ) ;
#10239 = AXIS2_PLACEMENT_3D ( 'NONE', #16499, #19949, #1796 ) ;
#10240 = CYLINDRICAL_SURFACE ( 'NONE', #1017, 10.00000000000000533 ) ;
#10241 = CARTESIAN_POINT ( 'NONE',  ( -40.53162694259542320, 234.1198905683720000, -11.84573899990672707 ) ) ;
#10242 = CARTESIAN_POINT ( 'NONE',  ( -10.76731745429010090, 56.85652257517428865, -46.25122601329427141 ) ) ;
#10243 = CARTESIAN_POINT ( 'NONE',  ( -36.33955658999049376, 225.3698905601784759, -18.47759065022572855 ) ) ;
#10244 = CARTESIAN_POINT ( 'NONE',  ( -38.17536295476244845, 272.3073905683720000, -14.20200298773971426 ) ) ;
#10245 = CARTESIAN_POINT ( 'NONE',  ( -13.20868407381886023, 360.9948905683720568, -6.410867750099233042 ) ) ;
#10246 = VECTOR ( 'NONE', #14358, 1000.000000000000000 ) ;
#10247 = CARTESIAN_POINT ( 'NONE',  ( -8.685887942688374608, 502.5573905601784759, -3.978247347592287486 ) ) ;
#10248 = AXIS2_PLACEMENT_3D ( 'NONE', #20906, #7587, #14215 ) ;
#10249 = CARTESIAN_POINT ( 'NONE',  ( -14.48388495494900496, 407.9323905683720000, 9.489475012073732785 ) ) ;
#10250 = CARTESIAN_POINT ( 'NONE',  ( -11.73070664223724791, 337.9323905765655809, -11.32908994701042538 ) ) ;
#10251 =( BOUNDED_CURVE ( )  B_SPLINE_CURVE ( 2, ( #9083, #18924, #8868, #18499, #18605, #17002, #3790, #18817, #4109, #13652, #3689, #7030, #17317, #10380, #3898, #8767, #13759 ),
 .UNSPECIFIED., .F., .T. ) 
 B_SPLINE_CURVE_WITH_KNOTS ( ( 3, 2, 2, 2, 2, 2, 2, 2, 3 ),
 ( 0.07812500000000043021, 0.08007812500000038858, 0.08203125000000034694, 0.08398437500000030531, 0.08593750000000024980, 0.08789062500000020817, 0.08984375000000016653, 0.09179687500000012490, 0.09375000000000008327 ),
 .UNSPECIFIED. ) 
 CURVE ( )  GEOMETRIC_REPRESENTATION_ITEM ( )  RATIONAL_B_SPLINE_CURVE ( ( 0.9999999999999957812, 0.9807852804032346494, 1.000000000000000000, 0.9807852804032304306, 1.000000000000000000, 0.9807852804032304306, 1.000000000000000000, 0.9807852804032304306, 1.000000000000000000, 0.9807852804032304306, 1.000000000000000000, 0.9807852804032304306, 1.000000000000000000, 0.9807852804032304306, 1.000000000000000000, 0.9807852804032296534, 1.000000000000000888 ) ) 
 REPRESENTATION_ITEM ( '' )  );
#10252 = CARTESIAN_POINT ( 'NONE',  ( -21.03221929538691626, 410.3698905601784759, 18.47759065022572500 ) ) ;
#10253 = ORIENTED_EDGE ( 'NONE', *, *, #2893, .F. ) ;
#10254 = DIRECTION ( 'NONE',  ( 0.000000000000000000, 1.000000000000000000, -0.000000000000000000 ) ) ;
#10255 = ORIENTED_EDGE ( 'NONE', *, *, #20031, .T. ) ;
#10256 = ORIENTED_EDGE ( 'NONE', *, *, #12606, .F. ) ;
#10257 = CARTESIAN_POINT ( 'NONE',  ( -16.84014894278201169, 531.6198905683720568, -11.84573899990672707 ) ) ;
#10258 = CARTESIAN_POINT ( 'NONE',  ( -10.20829729246297646, 282.8698905601784759, -7.653668647301794969 ) ) ;
#10259 = CARTESIAN_POINT ( 'NONE',  ( -43.66427838156418773, 210.0786766341574889, -0.8210443013742924068 ) ) ;
#10260 = ADVANCED_FACE ( 'NONE', ( #18471 ), #13622, .F. ) ;
#10261 = CARTESIAN_POINT ( 'NONE',  ( -25.35362745456397704, 328.1823905683720568, 16.75240474999998952 ) ) ;
#10262 = AXIS2_PLACEMENT_3D ( 'NONE', #10218, #4821, #1484 ) ;
#10263 = ORIENTED_EDGE ( 'NONE', *, *, #15717, .T. ) ;
#10264 = CARTESIAN_POINT ( 'NONE',  ( -44.16309181155856578, 354.4948905683720000, 6.410867750099241924 ) ) ;
#10265 = ADVANCED_FACE ( 'NONE', ( #19887 ), #11033, .T. ) ;
#10266 = CARTESIAN_POINT ( 'NONE',  ( -25.35362745456398059, 366.6823905683720568, 16.75240474999998952 ) ) ;
#10267 = ADVANCED_FACE ( 'NONE', ( #16659 ), #11560, .T. ) ;
#10268 = VECTOR ( 'NONE', #15702, 1000.000000000000000 ) ;
#10269 = CARTESIAN_POINT ( 'NONE',  ( -24.70764059509555466, 309.1823905765656377, -19.99999999999999289 ) ) ;
#10270 = DIRECTION ( 'NONE',  ( -1.191790137725560488E-16, 1.000000000000000000, -0.000000000000000000 ) ) ;
#10271 = CARTESIAN_POINT ( 'NONE',  ( -42.88789093042842637, 272.9323905683721136, -9.489475012073734561 ) ) ;
#10272 = CARTESIAN_POINT ( 'NONE',  ( -43.37470026482864682, 201.1699573972601343, 3.051950158715579065 ) ) ;
#10273 = CARTESIAN_POINT ( 'NONE',  ( -28.68588794268872277, 412.8698905683720568, -16.75240474999999307 ) ) ;
#10274 = DIRECTION ( 'NONE',  ( -1.191790137725560488E-16, 1.000000000000000000, -0.000000000000000000 ) ) ;
#10275 = CARTESIAN_POINT ( 'NONE',  ( -24.70764059509555821, 354.4323905601784759, -19.99999999999999289 ) ) ;
#10276 = CARTESIAN_POINT ( 'NONE',  ( -24.70764059509553690, 274.8073905765656377, 19.99999999999998934 ) ) ;
#10277 = CARTESIAN_POINT ( 'NONE',  ( -46.31968306282883674, 230.5765313837437418, 33.59072564020503648 ) ) ;
#10278 = EDGE_CURVE ( 'NONE', #5170, #17823, #6682, .T. ) ;
#10279 = CARTESIAN_POINT ( 'NONE',  ( -16.84014894278198682, 331.6198905683720000, -11.84573899990672707 ) ) ;
#10280 = CARTESIAN_POINT ( 'NONE',  ( -25.35362745456399125, 456.6823905683720000, 16.75240474999998952 ) ) ;
#10281 = VERTEX_POINT ( 'NONE', #3448 ) ;
#10282 = CARTESIAN_POINT ( 'NONE',  ( -10.20829729246299777, 471.6198905601784759, 7.653668647301790529 ) ) ;
#10283 = CARTESIAN_POINT ( 'NONE',  ( -13.20868407381885135, 279.4948905683720000, -6.410867750099233042 ) ) ;
#10284 = DIRECTION ( 'NONE',  ( -1.000000000000000000, 0.000000000000000000, 0.000000000000000000 ) ) ;
#10285 = VERTEX_POINT ( 'NONE', #1844 ) ;
#10286 = CARTESIAN_POINT ( 'NONE',  ( 166.1493775951145437, 620.7448905601785327, 8.917803138848105604 ) ) ;
#10287 = CARTESIAN_POINT ( 'NONE',  ( -28.68588794268871212, 344.7448905601784759, -19.99999999999999289 ) ) ;
#10288 = CARTESIAN_POINT ( 'NONE',  ( -22.27502019258949062, 392.2448905683720568, -15.47720386886985544 ) ) ;
#10289 = CARTESIAN_POINT ( 'NONE',  ( -8.685887942688706786, 232.2448905601785043, -2.449293598294705724E-15 ) ) ;
#10290 = CARTESIAN_POINT ( 'NONE',  ( -8.685887942688726326, 386.9948905765655809, -2.449293598294705724E-15 ) ) ;
#10291 = CARTESIAN_POINT ( 'NONE',  ( -16.84014894278199748, 420.1198905683720000, -11.84573899990672707 ) ) ;
#10292 = CARTESIAN_POINT ( 'NONE',  ( -45.43829269268869098, 265.6823905683720568, 3.332260488124734632 ) ) ;
#10293 = CARTESIAN_POINT ( 'NONE',  ( -11.93348319268872793, 418.8698905683720568, -2.051577885510841163E-15 ) ) ;
#10294 = CARTESIAN_POINT ( 'NONE',  ( -11.73070664223724791, 356.0573905765655809, 11.32908994701042005 ) ) ;
#10295 = CARTESIAN_POINT ( 'NONE',  ( -48.68588794268853803, 276.9323905601784759, -3.978247347593583783 ) ) ;
#10296 = CARTESIAN_POINT ( 'NONE',  ( -22.27502019258948351, 320.7448905683720000, -15.47720386886985544 ) ) ;
#10297 = CARTESIAN_POINT ( 'NONE',  ( -36.33955658999052218, 490.1198905765656377, -18.47759065022572855 ) ) ;
#10298 = CARTESIAN_POINT ( 'NONE',  ( -40.53162694259545162, 486.6198905683720000, 11.84573899990672885 ) ) ;
#10299 = DIRECTION ( 'NONE',  ( 0.000000000000000000, 0.000000000000000000, 1.000000000000000000 ) ) ;
#10300 = CARTESIAN_POINT ( 'NONE',  ( -43.04679578547634122, 202.6324317550694616, -4.335932898175371975 ) ) ;
#10301 = DIRECTION ( 'NONE',  ( 1.000000000000000000, 0.000000000000000000, -0.000000000000000000 ) ) ;
#10302 = CARTESIAN_POINT ( 'NONE',  ( -19.19641293061498999, 391.9323905683720000, -14.20200298773971603 ) ) ;
#10303 = CARTESIAN_POINT ( 'NONE',  ( -46.31968306282883674, 303.6587712403113528, 33.59072564020503648 ) ) ;
#10304 = CARTESIAN_POINT ( 'NONE',  ( -28.68588794268873698, 524.7448905601785327, -19.99999999999999289 ) ) ;
#10305 = CARTESIAN_POINT ( 'NONE',  ( -14.48388495494899963, 359.8073905683720000, -9.489475012073736337 ) ) ;
#10306 = CIRCLE ( 'NONE', #12031, 20.00000000000000711 ) ;
#10307 = ORIENTED_EDGE ( 'NONE', *, *, #7093, .F. ) ;
#10308 = CARTESIAN_POINT ( 'NONE',  ( -28.68588794268873343, 526.3698905683720568, 16.75240474999999307 ) ) ;
#10309 = VERTEX_POINT ( 'NONE', #13516 ) ;
#10310 = CARTESIAN_POINT ( 'NONE',  ( -8.685887942688720997, 352.2448905601784759, -2.449293598294705724E-15 ) ) ;
#10311 = CARTESIAN_POINT ( 'NONE',  ( -25.35362745456401257, 521.0573905683720568, -16.75240474999999307 ) ) ;
#10312 = VERTEX_POINT ( 'NONE', #10242 ) ;
#10313 = CARTESIAN_POINT ( 'NONE',  ( -14.54375231895778597, 493.4948905601784759, -14.14213562373094746 ) ) ;
#10314 = CARTESIAN_POINT ( 'NONE',  ( -28.68588794268872633, 476.3698905683720568, 16.75240474999999307 ) ) ;
#10315 = VERTEX_POINT ( 'NONE', #433 ) ;
#10316 = CARTESIAN_POINT ( 'NONE',  ( -11.93348319268873681, 488.8698905683720568, -2.051577885510841163E-15 ) ) ;
#10317 = CARTESIAN_POINT ( 'NONE',  ( -11.73070664223726212, 491.3073905601784759, 11.32908994701042005 ) ) ;
#10318 = EDGE_CURVE ( 'NONE', #16131, #19239, #1434, .T. ) ;
#10319 = CARTESIAN_POINT ( 'NONE',  ( -42.82802356641966668, 433.2448905765656377, 14.14213562373094923 ) ) ;
#10320 = CARTESIAN_POINT ( 'NONE',  ( -10.20829729246297823, 297.6198905765656377, -7.653668647301794969 ) ) ;
#10321 = DIRECTION ( 'NONE',  ( 0.000000000000000000, 0.000000000000000000, -1.000000000000000000 ) ) ;
#10322 = CARTESIAN_POINT ( 'NONE',  ( -36.33955658999051508, 440.1198905765656377, -18.47759065022572855 ) ) ;
#10323 = CARTESIAN_POINT ( 'NONE',  ( 154.7587007620219026, 610.7448905601785327, 10.81142786866622885 ) ) ;
#10324 = VECTOR ( 'NONE', #3502, 1000.000000000000000 ) ;
#10325 = CARTESIAN_POINT ( 'NONE',  ( 6.416697501590670427, 217.7548513357008630, 45.00000000000000000 ) ) ;
#10326 = EDGE_CURVE ( 'NONE', #17590, #11997, #17609, .T. ) ;
#10327 = CARTESIAN_POINT ( 'NONE',  ( 5.074999999999999289, -7.505553499465148271, 0.000000000000000000 ) ) ;
#10328 = CARTESIAN_POINT ( 'NONE',  ( -22.27502019258946930, 298.4948905683720568, 15.47720386886985189 ) ) ;
#10329 = FACE_OUTER_BOUND ( 'NONE', #19573, .T. ) ;
#10330 = CARTESIAN_POINT ( 'NONE',  ( -16.84014894278199748, 449.1198905683720568, 11.84573899990672530 ) ) ;
#10331 = CARTESIAN_POINT ( 'NONE',  ( -33.84809828339280102, 56.85652257517428865, -49.33155846391706945 ) ) ;
#10332 = CARTESIAN_POINT ( 'NONE',  ( -32.01814843081344009, 277.5573905683720000, 16.75240474999999307 ) ) ;
#10333 = VERTEX_POINT ( 'NONE', #18366 ) ;
#10334 = CARTESIAN_POINT ( 'NONE',  ( -17.35679799567827786, 270.6823905601785327, 16.95518130045146421 ) ) ;
#10335 = EDGE_CURVE ( 'NONE', #15878, #19602, #9443, .T. ) ;
#10336 = CARTESIAN_POINT ( 'NONE',  ( -19.19641293061499709, 498.8073905683720568, 14.20200298773971426 ) ) ;
#10337 = AXIS2_PLACEMENT_3D ( 'NONE', #11363, #3266, #11257 ) ;
#10338 = VERTEX_POINT ( 'NONE', #7171 ) ;
#10339 = CARTESIAN_POINT ( 'NONE',  ( -35.09675569278796559, 467.2448905683720568, 15.47720386886985366 ) ) ;
#10340 = CARTESIAN_POINT ( 'NONE',  ( 0.000000000000000000, 130.1716627696692683, -25.00000000000000000 ) ) ;
#10341 = CARTESIAN_POINT ( 'NONE',  ( -14.48388495494898542, 257.9323905683720568, 9.489475012073732785 ) ) ;
#10342 = VERTEX_POINT ( 'NONE', #15420 ) ;
#10343 = CARTESIAN_POINT ( 'NONE',  ( 115.7989814974898195, 160.1716627696691830, -40.00000000000000000 ) ) ;
#10344 = EDGE_CURVE ( 'NONE', #8850, #6325, #17039, .T. ) ;
#10345 = CARTESIAN_POINT ( 'NONE',  ( -32.01814843081343298, 267.5573905683720000, 16.75240474999999307 ) ) ;
#10346 = CARTESIAN_POINT ( 'NONE',  ( -36.33955658999052218, 490.1198905765656377, -18.47759065022572855 ) ) ;
#10347 = CARTESIAN_POINT ( 'NONE',  ( -21.03221929538691271, 390.3698905601785327, 18.47759065022572500 ) ) ;
#10348 = CARTESIAN_POINT ( 'NONE',  ( -28.68588794268869790, 247.8698905683720000, 16.75240474999999307 ) ) ;
#10349 = DIRECTION ( 'NONE',  ( 0.000000000000000000, 0.000000000000000000, 1.000000000000000000 ) ) ;
#10350 = CARTESIAN_POINT ( 'NONE',  ( -21.03221929538690915, 234.1198905601784475, -18.47759065022572855 ) ) ;
#10351 = CARTESIAN_POINT ( 'NONE',  ( -40.53162694259542320, 242.6198905683720284, -11.84573899990672707 ) ) ;
#10352 = CARTESIAN_POINT ( 'NONE',  ( -16.84014894278199037, 361.6198905683720000, -11.84573899990672707 ) ) ;
#10353 = CARTESIAN_POINT ( 'NONE',  ( 14.09825962131072785, 230.5765313837437418, 25.00000000000000000 ) ) ;
#10354 = EDGE_CURVE ( 'NONE', #18169, #4442, #2222, .T. ) ;
#10355 = CARTESIAN_POINT ( 'NONE',  ( -13.20868407381886556, 399.4948905683720000, -6.410867750099233042 ) ) ;
#10356 = CARTESIAN_POINT ( 'NONE',  ( -46.31968306282883674, 230.5765313837437418, 33.59072564020503648 ) ) ;
#10357 = CARTESIAN_POINT ( 'NONE',  ( -32.66413529028188378, 409.4323905601784759, 19.99999999999999289 ) ) ;
#10358 = EDGE_LOOP ( 'NONE', ( #3415, #7195 ) ) ;
#10359 = CARTESIAN_POINT ( 'NONE',  ( -28.68588794268871567, 349.4948905765656377, -19.99999999999999289 ) ) ;
#10360 = VERTEX_POINT ( 'NONE', #3937 ) ;
#10361 = VERTEX_POINT ( 'NONE', #8804 ) ;
#10362 = FACE_OUTER_BOUND ( 'NONE', #18220, .T. ) ;
#10363 = CARTESIAN_POINT ( 'NONE',  ( -36.33955658999050797, 289.1198905601785327, 18.47759065022572500 ) ) ;
#10364 = CARTESIAN_POINT ( 'NONE',  ( -10.20829729246298001, 317.6198905765655809, -7.653668647301794969 ) ) ;
#10365 = EDGE_CURVE ( 'NONE', #6110, #1587, #2258, .T. ) ;
#10366 = CARTESIAN_POINT ( 'NONE',  ( -45.43829269268870519, 315.0573905683720000, -3.332260488124726638 ) ) ;
#10367 = AXIS2_PLACEMENT_3D ( 'NONE', #1347, #13132, #14345 ) ;
#10368 = EDGE_LOOP ( 'NONE', ( #10154, #19681, #13910, #2429, #19114, #4473, #6305, #20890, #6083, #10984, #18278, #17772, #677, #19368, #17509, #18584, #3234, #9578, #10491, #21159, #8080, #12909, #4704, #15875, #4009, #9851, #13426, #20219, #16305, #5398, #4654, #9362, #16733, #9037, #9727, #6374, #13656, #5188, #1505, #10553, #1664, #10654, #5873, #7547, #14755, #7520, #8449, #20839, #19401, #21342, #16406, #1578, #19393, #21286, #20458, #9571, #12622, #8045, #10574, #8933, #3483, #3936, #6015, #2883, #13842 ) ) ;
#10369 = CARTESIAN_POINT ( 'NONE',  ( -32.01814843081344719, 341.6823905683720000, -16.75240474999999307 ) ) ;
#10370 = CARTESIAN_POINT ( 'NONE',  ( -16.84014894278198682, 357.6198905683720000, 11.84573899990672530 ) ) ;
#10371 = AXIS2_PLACEMENT_3D ( 'NONE', #2252, #10136, #2144 ) ;
#10372 = CARTESIAN_POINT ( 'NONE',  ( -10.20829729246297646, 276.3698905765656377, 7.653668647301790529 ) ) ;
#10373 = AXIS2_PLACEMENT_3D ( 'NONE', #359, #11367, #19593 ) ;
#10374 = CARTESIAN_POINT ( 'NONE',  ( 20.42502041961813575, 271.1055109169419666, 40.00000000000000000 ) ) ;
#10375 = CARTESIAN_POINT ( 'NONE',  ( -28.68588794268870146, 266.3698905683720000, 16.75240474999999307 ) ) ;
#10376 = CARTESIAN_POINT ( 'NONE',  ( -10.20829729246299777, 466.3698905765656377, 7.653668647301790529 ) ) ;
#10377 = CIRCLE ( 'NONE', #1086, 200.0000000000000000 ) ;
#10378 = CARTESIAN_POINT ( 'NONE',  ( -13.20868407381886556, 410.9948905683720000, -6.410867750099233042 ) ) ;
#10379 = FACE_OUTER_BOUND ( 'NONE', #5882, .T. ) ;
#10380 = CARTESIAN_POINT ( 'NONE',  ( -45.64106924314020119, 502.9323905765656946, 11.32908994701042538 ) ) ;
#10381 =( BOUNDED_CURVE ( )  B_SPLINE_CURVE ( 2, ( #17131, #10295, #20262, #18420, #16709, #15408, #16918, #5227, #7054, #20161, #13778, #6843, #2100, #5432, #18312, #12033, #8466 ),
 .UNSPECIFIED., .F., .T. ) 
 B_SPLINE_CURVE_WITH_KNOTS ( ( 3, 2, 2, 2, 2, 2, 2, 2, 3 ),
 ( 0.8125000000000002220, 0.8144531250000002220, 0.8164062500000002220, 0.8183593750000002220, 0.8203125000000002220, 0.8222656250000002220, 0.8242187500000002220, 0.8261718750000002220, 0.8281250000000002220 ),
 .UNSPECIFIED. ) 
 CURVE ( )  GEOMETRIC_REPRESENTATION_ITEM ( )  RATIONAL_B_SPLINE_CURVE ( ( 0.9999999999999977796, 0.9807852804032326510, 1.000000000000000000, 0.9807852804032304306, 1.000000000000000000, 0.9807852804032304306, 1.000000000000000000, 0.9807852804032304306, 1.000000000000000000, 0.9807852804032304306, 1.000000000000000000, 0.9807852804032304306, 1.000000000000000000, 0.9807852804032304306, 1.000000000000000000, 0.9807852804032282101, 1.000000000000002220 ) ) 
 REPRESENTATION_ITEM ( '' )  );
#10382 = DIRECTION ( 'NONE',  ( 0.000000000000000000, -1.000000000000000000, 0.000000000000000000 ) ) ;
#10383 = CARTESIAN_POINT ( 'NONE',  ( -35.09675569278794427, 285.7448905683720568, 15.47720386886985366 ) ) ;
#10384 = CARTESIAN_POINT ( 'NONE',  ( -28.68588794268871212, 322.8698905683720000, -16.75240474999999307 ) ) ;
#10385 = CARTESIAN_POINT ( 'NONE',  ( -11.93348319268873503, 468.8698905683720000, -2.051577885510841163E-15 ) ) ;
#10386 = ORIENTED_EDGE ( 'NONE', *, *, #12935, .F. ) ;
#10387 = CARTESIAN_POINT ( 'NONE',  ( -48.68588794268872277, 466.9323905601785327, -3.978247347593158345 ) ) ;
#10388 = CARTESIAN_POINT ( 'NONE',  ( -16.84014894278197971, 287.6198905683720000, 11.84573899990672530 ) ) ;
#10389 = AXIS2_PLACEMENT_3D ( 'NONE', #3601, #13451, #11606 ) ;
#10390 = CIRCLE ( 'NONE', #8618, 10.00000000000000888 ) ;
#10391 = ORIENTED_EDGE ( 'NONE', *, *, #1982, .F. ) ;
#10392 = DIRECTION ( 'NONE',  ( -0.000000000000000000, -0.000000000000000000, -1.000000000000000000 ) ) ;
#10393 = CARTESIAN_POINT ( 'NONE',  ( -47.16347859291444422, 337.8698905601785327, 7.653668647301805628 ) ) ;
#10394 = CARTESIAN_POINT ( 'NONE',  ( -16.84014894278197971, 307.6198905683720000, 11.84573899990672530 ) ) ;
#10395 = CARTESIAN_POINT ( 'NONE',  ( -35.09675569278795138, 377.2448905683720000, 15.47720386886985366 ) ) ;
#10396 = LINE ( 'NONE', #20574, #45 ) ;
#10397 = CARTESIAN_POINT ( 'NONE',  ( -47.16347859291446554, 522.6198905765655809, 7.653668647301805628 ) ) ;
#10398 = CARTESIAN_POINT ( 'NONE',  ( -32.01814843081345430, 411.6823905683720568, -16.75240474999999307 ) ) ;
#10399 = CARTESIAN_POINT ( 'NONE',  ( -32.01814843081343298, 267.5573905683720000, 16.75240474999999307 ) ) ;
#10400 = EDGE_CURVE ( 'NONE', #17320, #1920, #18965, .T. ) ;
#10401 = CARTESIAN_POINT ( 'NONE',  ( -22.27502019258948351, 416.9948905683720000, 15.47720386886985189 ) ) ;
#10402 = CONTEXT_DEPENDENT_SHAPE_REPRESENTATION ( #11095, #14615 ) ;
#10403 = ADVANCED_FACE ( 'NONE', ( #4043 ), #4447, .F. ) ;
#10404 = CARTESIAN_POINT ( 'NONE',  ( -42.82802356641965957, 370.7448905765656377, -14.14213562373094746 ) ) ;
#10405 = DIRECTION ( 'NONE',  ( -1.000000000000000000, 0.000000000000000000, -8.901024030850960568E-17 ) ) ;
#10406 = CARTESIAN_POINT ( 'NONE',  ( -44.16309181155855867, 324.4948905683720568, 6.410867750099241924 ) ) ;
#10407 = CARTESIAN_POINT ( 'NONE',  ( -32.01814843081346140, 477.5573905683720568, 16.75240474999999307 ) ) ;
#10408 = CARTESIAN_POINT ( 'NONE',  ( 6.416697501590670427, 172.9933428177121471, 45.00000000000000000 ) ) ;
#10409 = CARTESIAN_POINT ( 'NONE',  ( -42.93765923600280843, 203.3731313234725917, -4.678819197459183954 ) ) ;
#10410 = CARTESIAN_POINT ( 'NONE',  ( -24.70764059509552979, 224.8073905765656662, 19.99999999999998934 ) ) ;
#10411 = CARTESIAN_POINT ( 'NONE',  ( -11.93348319268872260, 380.6823905683720568, -3.332260488124732856 ) ) ;
#10412 = DIRECTION ( 'NONE',  ( 0.000000000000000000, 0.000000000000000000, 1.000000000000000000 ) ) ;
#10413 = CARTESIAN_POINT ( 'NONE',  ( -36.33955658999052929, 535.3698905601784190, -18.47759065022572855 ) ) ;
#10414 = CARTESIAN_POINT ( 'NONE',  ( -22.27502019258947286, 336.9948905683720000, 15.47720386886985189 ) ) ;
#10415 = VERTEX_POINT ( 'NONE', #10632 ) ;
#10416 = CARTESIAN_POINT ( 'NONE',  ( -13.20868407381887799, 518.2448905683720568, 6.410867750099229490 ) ) ;
#10417 = ORIENTED_EDGE ( 'NONE', *, *, #19479, .T. ) ;
#10418 = CARTESIAN_POINT ( 'NONE',  ( -14.54375231895776821, 353.4948905601785327, -14.14213562373094746 ) ) ;
#10419 = DIRECTION ( 'NONE',  ( 0.4627175328665442677, 0.000000000000000000, 0.8865057725575724579 ) ) ;
#10420 = CARTESIAN_POINT ( 'NONE',  ( 170.2047888904039610, 620.7448905601785327, -1.893624729818132124 ) ) ;
#10421 = CARTESIAN_POINT ( 'NONE',  ( -42.82802356641965247, 290.7448905765655809, -14.14213562373094746 ) ) ;
#10422 = CARTESIAN_POINT ( 'NONE',  ( -42.82802356641967378, 495.9948905601784759, -14.14213562373094746 ) ) ;
#10423 = CARTESIAN_POINT ( 'NONE',  ( -45.43829269268871940, 483.5573905683720000, -3.332260488124726194 ) ) ;
#10424 = CIRCLE ( 'NONE', #3871, 10.00000000000000888 ) ;
#10425 = ORIENTED_EDGE ( 'NONE', *, *, #4688, .F. ) ;
#10426 = CARTESIAN_POINT ( 'NONE',  ( -35.09675569278796559, 495.7448905683720000, 15.47720386886985366 ) ) ;
#10427 = CARTESIAN_POINT ( 'NONE',  ( -17.35679799567830273, 490.6823905601784190, 16.95518130045146421 ) ) ;
#10428 = CARTESIAN_POINT ( 'NONE',  ( -10.20829729246299244, 417.6198905765656377, -7.653668647301794969 ) ) ;
#10429 = DIRECTION ( 'NONE',  ( -0.000000000000000000, 1.000000000000000000, -0.000000000000000000 ) ) ;
#10430 = CARTESIAN_POINT ( 'NONE',  ( -8.685887942688736985, 486.9948905765656377, -2.449293598294705724E-15 ) ) ;
#10431 = CARTESIAN_POINT ( 'NONE',  ( -8.685887942688738761, 506.9948905765655240, -2.449293598294705724E-15 ) ) ;
#10432 = CARTESIAN_POINT ( 'NONE',  ( -8.685887942688848895, 486.6823905765656946, 3.978247347593427907 ) ) ;
#10433 = DIRECTION ( 'NONE',  ( -1.191790137725560488E-16, 1.000000000000000000, -0.000000000000000000 ) ) ;
#10434 = SURFACE_SIDE_STYLE ('',( #4163 ) ) ;
#10435 = DIRECTION ( 'NONE',  ( 1.000000000000000000, 1.374938938973709817E-16, -0.000000000000000000 ) ) ;
#10436 = AXIS2_PLACEMENT_3D ( 'NONE', #9131, #18652, #12284 ) ;
#10437 = CARTESIAN_POINT ( 'NONE',  ( -14.48388495494899075, 281.3073905683720000, -9.489475012073736337 ) ) ;
#10438 = CARTESIAN_POINT ( 'NONE',  ( -17.35679799567827786, 250.6823905601785043, 16.95518130045146421 ) ) ;
#10439 = DIRECTION ( 'NONE',  ( -0.000000000000000000, 0.5000000000000012212, 0.8660254037844380415 ) ) ;
#10440 = CARTESIAN_POINT ( 'NONE',  ( -13.20868407381887089, 440.9948905683720568, -6.410867750099233042 ) ) ;
#10441 = LINE ( 'NONE', #20516, #16481 ) ;
#10442 = CARTESIAN_POINT ( 'NONE',  ( -19.19641293061497223, 278.8073905683720000, 14.20200298773971426 ) ) ;
#10443 = ORIENTED_EDGE ( 'NONE', *, *, #10549, .T. ) ;
#10444 = PLANE ( 'NONE',  #5994 ) ;
#10445 = CARTESIAN_POINT ( 'NONE',  ( -32.01814843081345430, 493.1823905683721136, -16.75240474999999307 ) ) ;
#10446 = EDGE_CURVE ( 'NONE', #5712, #15685, #4556, .T. ) ;
#10447 = ORIENTED_EDGE ( 'NONE', *, *, #4778, .F. ) ;
#10448 = EDGE_CURVE ( 'NONE', #8661, #12838, #16035, .T. ) ;
#10449 = DIRECTION ( 'NONE',  ( 0.9283449136418786551, -0.000000000000000000, 0.3717199501173604204 ) ) ;
#10450 = CARTESIAN_POINT ( 'NONE',  ( -11.93348319268871016, 268.8698905683720000, -2.051577885510841163E-15 ) ) ;
#10451 = AXIS2_PLACEMENT_3D ( 'NONE', #9084, #12563, #5729 ) ;
#10452 = VERTEX_POINT ( 'NONE', #16136 ) ;
#10453 = CARTESIAN_POINT ( 'NONE',  ( 0.1061556211655396709, -6.421950209808290566, -1.876855952934453731 ) ) ;
#10454 = CARTESIAN_POINT ( 'NONE',  ( -28.68588794268872633, 484.4948905765656377, 19.99999999999999289 ) ) ;
#10455 = CARTESIAN_POINT ( 'NONE',  ( -40.01497788969913216, 388.8073905601784759, 16.95518130045146776 ) ) ;
#10456 = CARTESIAN_POINT ( 'NONE',  ( -22.27502019258947286, 242.2448905683720000, -15.47720386886985544 ) ) ;
#10457 = CARTESIAN_POINT ( 'NONE',  ( -42.88789093042845479, 514.4323905683720568, -9.489475012073736337 ) ) ;
#10458 = LINE ( 'NONE', #20746, #8717 ) ;
#10459 = CARTESIAN_POINT ( 'NONE',  ( -44.16309181155855867, 243.2448905683720000, -6.410867750099231266 ) ) ;
#10460 = CARTESIAN_POINT ( 'NONE',  ( -32.01814843081344719, 357.5573905683720000, 16.75240474999999307 ) ) ;
#10461 = AXIS2_PLACEMENT_3D ( 'NONE', #10046, #12319, #5818 ) ;
#10462 = CARTESIAN_POINT ( 'NONE',  ( -32.66413529028186247, 279.4323905601785327, 19.99999999999999289 ) ) ;
#10463 = EDGE_CURVE ( 'NONE', #661, #9549, #7890, .T. ) ;
#10464 = CARTESIAN_POINT ( 'NONE',  ( -11.93348319268872615, 409.1823905683720568, -3.332260488124732856 ) ) ;
#10465 = DIRECTION ( 'NONE',  ( 1.000000000000000000, 0.000000000000000000, 0.000000000000000000 ) ) ;
#10466 = CARTESIAN_POINT ( 'NONE',  ( -24.70764059509556887, 414.4323905601785327, -19.99999999999999289 ) ) ;
#10467 = EDGE_LOOP ( 'NONE', ( #17949, #14537, #1110, #12379, #19960, #13877, #13590 ) ) ;
#10468 = FACE_BOUND ( 'NONE', #5054, .T. ) ;
#10469 = EDGE_LOOP ( 'NONE', ( #20940, #6930, #4142, #5693 ) ) ;
#10470 = ORIENTED_EDGE ( 'NONE', *, *, #14529, .T. ) ;
#10471 = CARTESIAN_POINT ( 'NONE',  ( -22.27502019258950483, 532.2448905683720568, -15.47720386886985544 ) ) ;
#10472 = CARTESIAN_POINT ( 'NONE',  ( -10.20829729246297646, 292.8698905601784759, -7.653668647301794969 ) ) ;
#10473 = LINE ( 'NONE', #13639, #9385 ) ;
#10474 = ORIENTED_EDGE ( 'NONE', *, *, #18466, .F. ) ;
#10475 = CIRCLE ( 'NONE', #4623, 4.000000000000003553 ) ;
#10476 = CARTESIAN_POINT ( 'NONE',  ( -16.84014894278198682, 331.6198905683720000, -11.84573899990672707 ) ) ;
#10477 = CARTESIAN_POINT ( 'NONE',  ( -11.93348319268872260, 349.1823905683720000, -3.332260488124732856 ) ) ;
#10478 = CARTESIAN_POINT ( 'NONE',  ( -14.48388495494900141, 369.8073905683720000, -9.489475012073734561 ) ) ;
#10479 = VECTOR ( 'NONE', #4312, 1000.000000000000114 ) ;
#10480 = EDGE_CURVE ( 'NONE', #4289, #20822, #8321, .T. ) ;
#10481 = CARTESIAN_POINT ( 'NONE',  ( -28.68588794268870146, 284.4948905765656377, 19.99999999999999289 ) ) ;
#10482 = DIRECTION ( 'NONE',  ( 1.000000000000000000, 0.000000000000000000, -8.901024030850963034E-17 ) ) ;
#10483 = CARTESIAN_POINT ( 'NONE',  ( -44.16309181155856578, 273.2448905683720568, -6.410867750099231266 ) ) ;
#10484 = CARTESIAN_POINT ( 'NONE',  ( -32.01814843081345430, 427.5573905683720000, 16.75240474999999307 ) ) ;
#10485 = CARTESIAN_POINT ( 'NONE',  ( -30.95117587177153951, 49.20052347319550989, 121.1077492336972909 ) ) ;
#10486 = PLANE ( 'NONE',  #10732 ) ;
#10487 = DIRECTION ( 'NONE',  ( -1.000000000000000000, 0.000000000000000000, 0.000000000000000000 ) ) ;
#10488 = ADVANCED_FACE ( 'NONE', ( #11463 ), #18062, .T. ) ;
#10489 = CARTESIAN_POINT ( 'NONE',  ( -40.53162694259543031, 326.6198905683720568, 11.84573899990672885 ) ) ;
#10490 = CARTESIAN_POINT ( 'NONE',  ( -19.19641293061498999, 457.3073905683720568, 14.20200298773971426 ) ) ;
#10491 = ORIENTED_EDGE ( 'NONE', *, *, #7877, .F. ) ;
#10492 = CARTESIAN_POINT ( 'NONE',  ( -24.70764059509556176, 460.0573905601784759, 19.99999999999998934 ) ) ;
#10493 = CARTESIAN_POINT ( 'NONE',  ( -40.53162694259543031, 285.1198905683720568, 11.84573899990672885 ) ) ;
#10494 = AXIS2_PLACEMENT_3D ( 'NONE', #158, #18192, #21235 ) ;
#10495 = ORIENTED_EDGE ( 'NONE', *, *, #4464, .F. ) ;
#10496 = CARTESIAN_POINT ( 'NONE',  ( -28.68588794268870856, 339.7448905601784759, 19.99999999999999289 ) ) ;
#10497 = CARTESIAN_POINT ( 'NONE',  ( -25.35362745456399125, 448.1823905683720000, 16.75240474999998952 ) ) ;
#10498 = VERTEX_POINT ( 'NONE', #14628 ) ;
#10499 = FACE_OUTER_BOUND ( 'NONE', #20414, .T. ) ;
#10500 = CARTESIAN_POINT ( 'NONE',  ( -17.35679799567829562, 343.8073905601785327, -16.95518130045146421 ) ) ;
#10501 = CARTESIAN_POINT ( 'NONE',  ( -35.09675569278793716, 291.9948905683720000, -15.47720386886985544 ) ) ;
#10502 = CARTESIAN_POINT ( 'NONE',  ( -40.53162694259543741, 376.6198905683720568, 11.84573899990672885 ) ) ;
#10503 = CARTESIAN_POINT ( 'NONE',  ( -8.685887942688738761, 512.2448905601784190, -2.449293598294705724E-15 ) ) ;
#10504 = CARTESIAN_POINT ( 'NONE',  ( -36.33955658999052929, 520.1198905765655809, -18.47759065022572855 ) ) ;
#10505 = CARTESIAN_POINT ( 'NONE',  ( -13.20868407381886378, 398.2448905683720568, 6.410867750099229490 ) ) ;
#10506 = CARTESIAN_POINT ( 'NONE',  ( -22.27502019258947286, 232.2448905683720000, -15.47720386886985544 ) ) ;
#10507 = CARTESIAN_POINT ( 'NONE',  ( -38.17536295476245556, 435.4323905683720568, 14.20200298773971781 ) ) ;
#10508 = CARTESIAN_POINT ( 'NONE',  ( -36.33955658999051508, 333.8698905765656377, 18.47759065022572500 ) ) ;
#10509 = CARTESIAN_POINT ( 'NONE',  ( 151.0910679931202196, 610.7448905601785327, 6.352526299242177821 ) ) ;
#10510 = CARTESIAN_POINT ( 'NONE',  ( -38.17536295476244845, 322.3073905683720568, -14.20200298773971426 ) ) ;
#10511 = CARTESIAN_POINT ( 'NONE',  ( -25.35362745456400546, 482.5573905683720000, -16.75240474999999307 ) ) ;
#10512 = LINE ( 'NONE', #17135, #15122 ) ;
#10513 = LINE ( 'NONE', #10728, #14220 ) ;
#10514 = CARTESIAN_POINT ( 'NONE',  ( 0.000000000000000000, 0.000000000000000000, 0.000000000000000000 ) ) ;
#10515 = CARTESIAN_POINT ( 'NONE',  ( -45.43829269268870519, 385.6823905683720000, 3.332260488124734632 ) ) ;
#10516 = DIRECTION ( 'NONE',  ( 0.000000000000000000, 0.000000000000000000, 1.000000000000000000 ) ) ;
#10517 = EDGE_CURVE ( 'NONE', #15177, #20201, #19386, .T. ) ;
#10518 = CARTESIAN_POINT ( 'NONE',  ( -48.68588794268872988, 526.9323905601785327, -3.978247347593158345 ) ) ;
#10519 = CARTESIAN_POINT ( 'NONE',  ( -44.16309181155856578, 344.4948905683720000, 6.410867750099241924 ) ) ;
#10520 = VERTEX_POINT ( 'NONE', #6377 ) ;
#10521 = CARTESIAN_POINT ( 'NONE',  ( -13.20868407381887799, 499.4948905683720568, -6.410867750099233042 ) ) ;
#10522 = ORIENTED_EDGE ( 'NONE', *, *, #1836, .F. ) ;
#10523 = CARTESIAN_POINT ( 'NONE',  ( -39.39453070547082802, 223.9102039777117170, -12.89991794593033525 ) ) ;
#10524 = CARTESIAN_POINT ( 'NONE',  ( 81.24038404635966515, -343.0245277843623057, -94.99999999999994316 ) ) ;
#10525 = CARTESIAN_POINT ( 'NONE',  ( -48.68588794268860909, 291.6823905765655809, -3.978247347593371508 ) ) ;
#10526 = CARTESIAN_POINT ( 'NONE',  ( -47.16347859291446554, 521.3698905765655809, -7.653668647301793193 ) ) ;
#10527 = CARTESIAN_POINT ( 'NONE',  ( -16.84014894278200458, 470.1198905683720568, -11.84573899990672707 ) ) ;
#10528 = ORIENTED_EDGE ( 'NONE', *, *, #2692, .T. ) ;
#10529 = CARTESIAN_POINT ( 'NONE',  ( -14.48388495494901385, 489.8073905683720568, -9.489475012073734561 ) ) ;
#10530 = CARTESIAN_POINT ( 'NONE',  ( -10.20829729246297291, 251.6198905601784759, 7.653668647301790529 ) ) ;
#10531 = ADVANCED_FACE ( 'NONE', ( #1748, #1638, #129 ), #13099, .T. ) ;
#10532 = CARTESIAN_POINT ( 'NONE',  ( -14.54375231895777176, 405.7448905765656377, 14.14213562373094568 ) ) ;
#10533 = CARTESIAN_POINT ( 'NONE',  ( -47.16347859291445843, 472.6198905765656377, 7.653668647301805628 ) ) ;
#10534 = CARTESIAN_POINT ( 'NONE',  ( 35.96497763894178945, 170.1716627696692683, -40.00000000000000000 ) ) ;
#10535 = CARTESIAN_POINT ( 'NONE',  ( -21.03221929538693757, 484.1198905601785327, -18.47759065022572855 ) ) ;
#10536 = CARTESIAN_POINT ( 'NONE',  ( 5.674999999999999822, 3.752776749732562589, 6.500000000000000000 ) ) ;
#10537 = EDGE_CURVE ( 'NONE', #17482, #1165, #9943, .T. ) ;
#10538 = ADVANCED_FACE ( 'NONE', ( #3043 ), #12889, .T. ) ;
#10539 = DIRECTION ( 'NONE',  ( -1.000000000000000000, 0.000000000000000000, 0.000000000000000000 ) ) ;
#10540 = DIRECTION ( 'NONE',  ( 0.000000000000000000, 1.000000000000000000, 0.000000000000000000 ) ) ;
#10541 = CARTESIAN_POINT ( 'NONE',  ( -123.2946569474810161, 30.52886280891152282, 20.57735571454641388 ) ) ;
#10542 = CARTESIAN_POINT ( 'NONE',  ( -14.48388495494898898, 271.3073905683720568, -9.489475012073736337 ) ) ;
#10543 = CARTESIAN_POINT ( 'NONE',  ( -48.68588794268869435, 246.9323905601784759, -3.978247347593158345 ) ) ;
#10544 = CARTESIAN_POINT ( 'NONE',  ( -28.68588794268871212, 364.4948905765656377, 19.99999999999999289 ) ) ;
#10545 = B_SPLINE_CURVE_WITH_KNOTS ( 'NONE', 3,
 ( #11833, #6745, #17999, #6634, #18428, #9985, #3194, #1572, #14772, #11727, #5019, #1798, #13361, #18320, #10095, #16717, #8474, #1906, #15097, #6850 ),
 .UNSPECIFIED., .F., .F.,
 ( 4, 2, 2, 2, 2, 2, 2, 2, 2, 4 ),
 ( 0.007875367097399143743, 0.008859169463295337929, 0.009842971829191533850, 0.01082677419508772804, 0.01181057656098392222, 0.01279437892688011814, 0.01377818129277631233, 0.01476198365867250825, 0.01525388484162060534, 0.01574578602456870244 ),
 .UNSPECIFIED. ) ;
#10546 = CARTESIAN_POINT ( 'NONE',  ( -22.27502019258948707, 438.4948905683720568, 15.47720386886985189 ) ) ;
#10547 = CARTESIAN_POINT ( 'NONE',  ( -45.64106924314017988, 331.0573905765655809, -11.32908994701042538 ) ) ;
#10548 = CARTESIAN_POINT ( 'NONE',  ( -25.35362745456396993, 278.1823905683720000, 16.75240474999998952 ) ) ;
#10549 = EDGE_CURVE ( 'NONE', #9177, #10520, #12834, .T. ) ;
#10550 = ORIENTED_EDGE ( 'NONE', *, *, #13867, .F. ) ;
#10551 = VERTEX_POINT ( 'NONE', #8212 ) ;
#10552 = CARTESIAN_POINT ( 'NONE',  ( -25.35362745456400901, 492.5573905683721136, -16.75240474999999307 ) ) ;
#10553 = ORIENTED_EDGE ( 'NONE', *, *, #13854, .F. ) ;
#10554 = CARTESIAN_POINT ( 'NONE',  ( -28.68588794268874054, 573.2448905601785327, 0.000000000000000000 ) ) ;
#10555 = CARTESIAN_POINT ( 'NONE',  ( -11.93348319268870661, 248.8698905683720000, -2.051577885510841163E-15 ) ) ;
#10556 = ORIENTED_EDGE ( 'NONE', *, *, #16983, .T. ) ;
#10557 = LINE ( 'NONE', #12408, #15259 ) ;
#10558 = CARTESIAN_POINT ( 'NONE',  ( -40.01497788969915348, 490.4323905765655809, -16.95518130045146421 ) ) ;
#10559 = CARTESIAN_POINT ( 'NONE',  ( -32.66413529028186957, 389.4323905601784759, 19.99999999999999289 ) ) ;
#10560 = CARTESIAN_POINT ( 'NONE',  ( -47.16347859291445843, 456.6198905601784759, -7.653668647301793193 ) ) ;
#10561 = CARTESIAN_POINT ( 'NONE',  ( -16.84014894278196905, 229.1198905683720000, 11.84573899990672530 ) ) ;
#10562 = CARTESIAN_POINT ( 'NONE',  ( -32.01814843081346851, 523.1823905683720568, -16.75240474999999307 ) ) ;
#10563 = CARTESIAN_POINT ( 'NONE',  ( 0.2578475836320711090, 6.890627091270371984, 1.065083781909172744 ) ) ;
#10564 = CARTESIAN_POINT ( 'NONE',  ( -14.48388495494898365, 247.9323905683720284, 9.489475012073732785 ) ) ;
#10565 = CARTESIAN_POINT ( 'NONE',  ( -40.53162694259543741, 344.1198905683720568, -11.84573899990672707 ) ) ;
#10566 = CARTESIAN_POINT ( 'NONE',  ( -21.03221929538690560, 320.3698905601785327, 18.47759065022572500 ) ) ;
#10567 = VECTOR ( 'NONE', #17918, 1000.000000000000000 ) ;
#10568 = CARTESIAN_POINT ( 'NONE',  ( -16.84014894278199392, 400.1198905683720000, -11.84573899990672707 ) ) ;
#10569 = CARTESIAN_POINT ( 'NONE',  ( -45.64106924314017277, 322.9323905765655809, 11.32908994701042538 ) ) ;
#10570 = CARTESIAN_POINT ( 'NONE',  ( -17.35679799567829562, 380.6823905601784759, 16.95518130045146421 ) ) ;
#10571 = VECTOR ( 'NONE', #14055, 1000.000000000000000 ) ;
#10572 = EDGE_LOOP ( 'NONE', ( #16853, #10237, #15794, #12099 ) ) ;
#10573 = DIRECTION ( 'NONE',  ( -1.000000000000000000, 0.000000000000000000, 0.000000000000000000 ) ) ;
#10574 = ORIENTED_EDGE ( 'NONE', *, *, #18795, .F. ) ;
#10575 = ORIENTED_EDGE ( 'NONE', *, *, #6299, .T. ) ;
#10576 = CARTESIAN_POINT ( 'NONE',  ( -45.43829269268872650, 505.3698905683721136, 0.000000000000000000 ) ) ;
#10577 = CARTESIAN_POINT ( 'NONE',  ( -8.685887942688717445, 316.9948905765655809, -2.449293598294705724E-15 ) ) ;
#10578 = ORIENTED_EDGE ( 'NONE', *, *, #15983, .F. ) ;
#10579 = CARTESIAN_POINT ( 'NONE',  ( -16.84014894278197971, 309.1198905683720000, 11.84573899990672530 ) ) ;
#10580 = ORIENTED_EDGE ( 'NONE', *, *, #2055, .F. ) ;
#10581 = CARTESIAN_POINT ( 'NONE',  ( -45.43829269268870519, 354.1823905683721136, 3.332260488124734632 ) ) ;
#10582 = CARTESIAN_POINT ( 'NONE',  ( -45.43829269268871229, 353.8698905683720568, 0.000000000000000000 ) ) ;
#10583 = EDGE_CURVE ( 'NONE', #7305, #4929, #21212, .T. ) ;
#10584 = AXIS2_PLACEMENT_3D ( 'NONE', #12291, #525, #5472 ) ;
#10585 = CARTESIAN_POINT ( 'NONE',  ( -40.01497788969912506, 283.5573905765655809, 16.95518130045146776 ) ) ;
#10586 = CARTESIAN_POINT ( 'NONE',  ( -40.01497788969915348, 500.4323905765656377, -16.95518130045146421 ) ) ;
#10587 = CARTESIAN_POINT ( 'NONE',  ( -42.88789093042841927, 242.9323905683720000, -9.489475012073734561 ) ) ;
#10588 = CARTESIAN_POINT ( 'NONE',  ( -14.54375231895777887, 465.7448905765655809, 14.14213562373094568 ) ) ;
#10589 = CARTESIAN_POINT ( 'NONE',  ( -45.43829269268871229, 405.0573905683721136, -3.332260488124726194 ) ) ;
#10590 = AXIS2_PLACEMENT_3D ( 'NONE', #3924, #6954, #10299 ) ;
#10591 = CARTESIAN_POINT ( 'NONE',  ( -48.68588794268870146, 277.2448905601784759, 0.000000000000000000 ) ) ;
#10592 = CARTESIAN_POINT ( 'NONE',  ( -21.03221929538692336, 354.1198905601785327, -18.47759065022572855 ) ) ;
#10593 = DIRECTION ( 'NONE',  ( -0.3512089204514986518, 0.000000000000000000, 0.9362971185447986899 ) ) ;
#10594 = CARTESIAN_POINT ( 'NONE',  ( -14.48388495494899431, 311.3073905683720568, -9.489475012073736337 ) ) ;
#10595 = CARTESIAN_POINT ( 'NONE',  ( -40.53162694259545162, 465.1198905683720568, 11.84573899990672885 ) ) ;
#10596 = EDGE_LOOP ( 'NONE', ( #4290, #17664 ) ) ;
#10597 = CARTESIAN_POINT ( 'NONE',  ( -21.03221929538692336, 470.3698905601784759, 18.47759065022572500 ) ) ;
#10598 = CARTESIAN_POINT ( 'NONE',  ( -35.09675569278794427, 285.7448905683720568, 15.47720386886985366 ) ) ;
#10599 = ADVANCED_FACE ( 'NONE', ( #16 ), #8340, .T. ) ;
#10600 = AXIS2_PLACEMENT_3D ( 'NONE', #14876, #1458, #16710 ) ;
#10601 = ORIENTED_EDGE ( 'NONE', *, *, #17374, .F. ) ;
#10602 = CARTESIAN_POINT ( 'NONE',  ( -48.68588794268887199, 337.5573905601784190, 3.978247347592742678 ) ) ;
#10603 = EDGE_LOOP ( 'NONE', ( #8666, #6037, #20525, #4656, #10897, #19218 ) ) ;
#10604 = ORIENTED_EDGE ( 'NONE', *, *, #13849, .T. ) ;
#10605 = CARTESIAN_POINT ( 'NONE',  ( 0.000000000000000000, 5.629165124598846326, -3.250000000000007550 ) ) ;
#10606 = CARTESIAN_POINT ( 'NONE',  ( -32.66413529028187668, 345.0573905601784759, -19.99999999999999289 ) ) ;
#10607 = CARTESIAN_POINT ( 'NONE',  ( -32.01814843081344009, 306.0573905683720000, 16.75240474999999307 ) ) ;
#10608 = VECTOR ( 'NONE', #20883, 1000.000000000000114 ) ;
#10609 = CARTESIAN_POINT ( 'NONE',  ( -35.09675569278795138, 393.4948905683720000, -15.47720386886985544 ) ) ;
#10610 = LINE ( 'NONE', #5426, #13509 ) ;
#10611 = CARTESIAN_POINT ( 'NONE',  ( -47.16347859291446554, 521.3698905765655809, -7.653668647301793193 ) ) ;
#10612 = CARTESIAN_POINT ( 'NONE',  ( -42.88789093042844058, 394.8073905683720000, 9.489475012073736337 ) ) ;
#10613 = CARTESIAN_POINT ( 'NONE',  ( -13.20868407381884602, 249.7448905683720000, 6.410867750099229490 ) ) ;
#10614 = CARTESIAN_POINT ( 'NONE',  ( -22.27502019258949417, 410.7448905683720568, -15.47720386886985544 ) ) ;
#10615 = CONTEXT_DEPENDENT_SHAPE_REPRESENTATION ( #478, #9406 ) ;
#10616 = EDGE_CURVE ( 'NONE', #364, #14788, #19795, .T. ) ;
#10617 = CARTESIAN_POINT ( 'NONE',  ( -42.82802356641965957, 340.7448905765655809, -14.14213562373094746 ) ) ;
#10618 = LINE ( 'NONE', #2417, #3430 ) ;
#10619 = CARTESIAN_POINT ( 'NONE',  ( -11.93348319268871549, 308.5573905683719431, 3.332260488124728859 ) ) ;
#10620 = CARTESIAN_POINT ( 'NONE',  ( -13.20868407381887444, 470.9948905683720000, -6.410867750099233042 ) ) ;
#10621 = CARTESIAN_POINT ( 'NONE',  ( -14.54375231895778597, 515.7448905765655809, 14.14213562373094568 ) ) ;
#10622 = CARTESIAN_POINT ( 'NONE',  ( 5.700000000000000178, 0.000000000000000000, 4.000000000000000000 ) ) ;
#10623 = CARTESIAN_POINT ( 'NONE',  ( -28.68588794268870856, 304.7448905601785327, -19.99999999999999289 ) ) ;
#10624 = CARTESIAN_POINT ( 'NONE',  ( -22.27502019258949062, 392.2448905683720568, -15.47720386886985544 ) ) ;
#10625 = CARTESIAN_POINT ( 'NONE',  ( -28.68588794268872633, 378.8848358243226357, 0.000000000000000000 ) ) ;
#10626 = CARTESIAN_POINT ( 'NONE',  ( -11.73070664223726922, 523.1823905601784190, -11.32908994701042715 ) ) ;
#10627 = CARTESIAN_POINT ( 'NONE',  ( -35.09675569278795138, 335.7448905683720568, 15.47720386886985366 ) ) ;
#10628 = ORIENTED_EDGE ( 'NONE', *, *, #4648, .F. ) ;
#10629 = CARTESIAN_POINT ( 'NONE',  ( -44.16309181155857999, 504.4948905683720568, 6.410867750099241924 ) ) ;
#10630 = ORIENTED_EDGE ( 'NONE', *, *, #6378, .T. ) ;
#10631 = CARTESIAN_POINT ( 'NONE',  ( -10.20829729246298356, 352.8698905601784759, -7.653668647301794969 ) ) ;
#10632 = CARTESIAN_POINT ( 'NONE',  ( -64.27068722059111394, 600.7448905601785327, 35.12437985717896538 ) ) ;
#10633 = DIRECTION ( 'NONE',  ( -0.000000000000000000, -1.000000000000000000, -0.000000000000000000 ) ) ;
#10634 = CARTESIAN_POINT ( 'NONE',  ( -28.68588794268872633, 271.1055109169419666, 0.000000000000000000 ) ) ;
#10635 = CARTESIAN_POINT ( 'NONE',  ( -24.70764059509557953, 519.1823905765655809, -19.99999999999999289 ) ) ;
#10636 = CARTESIAN_POINT ( 'NONE',  ( -28.68588794268872633, 466.3698905683720000, 16.75240474999999307 ) ) ;
#10637 = EDGE_LOOP ( 'NONE', ( #16883, #9755, #4475, #3385 ) ) ;
#10638 = CARTESIAN_POINT ( 'NONE',  ( -19.19641293061499354, 477.3073905683720000, 14.20200298773971426 ) ) ;
#10639 = DIRECTION ( 'NONE',  ( 1.191790137725560488E-16, -1.000000000000000000, -0.000000000000000000 ) ) ;
#10640 = CARTESIAN_POINT ( 'NONE',  ( -40.01497788969913927, 403.5573905765656946, 16.95518130045146776 ) ) ;
#10641 = FACE_OUTER_BOUND ( 'NONE', #17360, .T. ) ;
#10642 = LINE ( 'NONE', #17155, #19247 ) ;
#10643 = CARTESIAN_POINT ( 'NONE',  ( -48.68588794268872988, 531.9948905765656946, 0.000000000000000000 ) ) ;
#10644 = FACE_OUTER_BOUND ( 'NONE', #11489, .T. ) ;
#10645 = DIRECTION ( 'NONE',  ( 0.000000000000000000, -1.000000000000000000, 0.000000000000000000 ) ) ;
#10646 = CARTESIAN_POINT ( 'NONE',  ( -45.43829269268869808, 285.0573905683720000, -3.332260488124726194 ) ) ;
#10647 = CIRCLE ( 'NONE', #20685, 4.000000000000001776 ) ;
#10648 = CARTESIAN_POINT ( 'NONE',  ( -42.82802356641964536, 245.9948905601784759, -14.14213562373094746 ) ) ;
#10649 = CARTESIAN_POINT ( 'NONE',  ( -40.01497788969913927, 403.5573905765656946, 16.95518130045146776 ) ) ;
#10650 = CARTESIAN_POINT ( 'NONE',  ( -44.16309181155857999, 444.7448905683720000, -6.410867750099231266 ) ) ;
#10651 = CARTESIAN_POINT ( 'NONE',  ( -10.20829729246298179, 327.6198905765656377, -7.653668647301794969 ) ) ;
#10652 = CARTESIAN_POINT ( 'NONE',  ( -40.53162694259543031, 276.6198905683720568, 11.84573899990672885 ) ) ;
#10653 = ORIENTED_EDGE ( 'NONE', *, *, #2752, .T. ) ;
#10654 = ORIENTED_EDGE ( 'NONE', *, *, #7630, .F. ) ;
#10655 = CARTESIAN_POINT ( 'NONE',  ( -19.19641293061499709, 481.9323905683720000, -14.20200298773971603 ) ) ;
#10656 = ADVANCED_FACE ( 'NONE', ( #11576 ), #18167, .F. ) ;
#10657 = AXIS2_PLACEMENT_3D ( 'NONE', #1310, #16027, #16448 ) ;
#10658 = ORIENTED_EDGE ( 'NONE', *, *, #21202, .F. ) ;
#10659 = CARTESIAN_POINT ( 'NONE',  ( -48.68588794268843145, 366.9323905601784190, -3.978247347593797389 ) ) ;
#10660 = CARTESIAN_POINT ( 'NONE',  ( -11.93348319268870839, 248.5573905683719715, 3.332260488124728415 ) ) ;
#10661 = ORIENTED_EDGE ( 'NONE', *, *, #1971, .F. ) ;
#10662 = FACE_OUTER_BOUND ( 'NONE', #15140, .T. ) ;
#10663 = CIRCLE ( 'NONE', #15184, 49.93977357075243617 ) ;
#10664 = CARTESIAN_POINT ( 'NONE',  ( -48.68588794268872277, 471.9948905765656377, 0.000000000000000000 ) ) ;
#10665 = CARTESIAN_POINT ( 'NONE',  ( -8.685887942688539809, 307.3073905765654672, -3.978247347592740013 ) ) ;
#10666 = CARTESIAN_POINT ( 'NONE',  ( -21.03221929538693402, 454.1198905601784759, -18.47759065022572855 ) ) ;
#10667 = CARTESIAN_POINT ( 'NONE',  ( -13.20868407381884602, 230.9948905683720284, -6.410867750099233042 ) ) ;
#10668 = ADVANCED_FACE ( 'NONE', ( #4977 ), #7995, .T. ) ;
#10669 = CARTESIAN_POINT ( 'NONE',  ( -38.17536295476247687, 523.8073905683720568, -14.20200298773971426 ) ) ;
#10670 = CARTESIAN_POINT ( 'NONE',  ( 0.01372220897661636727, 5.948365447239582160, 2.697128823393878161 ) ) ;
#10671 = CARTESIAN_POINT ( 'NONE',  ( -19.19641293061496867, 247.3073905683720284, 14.20200298773971426 ) ) ;
#10672 = CARTESIAN_POINT ( 'NONE',  ( -45.43829269268870519, 335.6823905683720568, 3.332260488124734632 ) ) ;
#10673 = CARTESIAN_POINT ( 'NONE',  ( -14.54375231895777887, 470.9948905601784759, 14.14213562373094568 ) ) ;
#10674 = CARTESIAN_POINT ( 'NONE',  ( -40.01497788969913216, 358.8073905601784190, 16.95518130045146776 ) ) ;
#10675 = AXIS2_PLACEMENT_3D ( 'NONE', #1974, #13430, #18494 ) ;
#10676 = CARTESIAN_POINT ( 'NONE',  ( -38.17536295476244845, 375.4323905683720568, 14.20200298773971781 ) ) ;
#10677 = DIRECTION ( 'NONE',  ( 1.000000000000000000, 0.000000000000000000, -0.000000000000000000 ) ) ;
#10678 = CARTESIAN_POINT ( 'NONE',  ( -28.68588794268871567, 389.7448905601785327, 19.99999999999999289 ) ) ;
#10679 = ORIENTED_EDGE ( 'NONE', *, *, #453, .T. ) ;
#10680 = FACE_OUTER_BOUND ( 'NONE', #20761, .T. ) ;
#10681 = EDGE_LOOP ( 'NONE', ( #20783, #18719, #6755, #14065, #19958, #20700, #17046 ) ) ;
#10682 = ORIENTED_EDGE ( 'NONE', *, *, #12490, .F. ) ;
#10683 = CARTESIAN_POINT ( 'NONE',  ( -14.48388495494901562, 509.4323905683719431, 9.489475012073732785 ) ) ;
#10684 = DIRECTION ( 'NONE',  ( 0.000000000000000000, 0.000000000000000000, 1.000000000000000000 ) ) ;
#10685 = VERTEX_POINT ( 'NONE', #11249 ) ;
#10686 = CARTESIAN_POINT ( 'NONE',  ( -11.93348319268871549, 310.6823905683720568, -3.332260488124732856 ) ) ;
#10687 = VERTEX_POINT ( 'NONE', #12987 ) ;
#10688 = CARTESIAN_POINT ( 'NONE',  ( -19.19641293061498644, 350.4323905683720000, -14.20200298773971603 ) ) ;
#10689 = CARTESIAN_POINT ( 'NONE',  ( -28.68588794268871567, 351.3698905683720568, -16.75240474999999307 ) ) ;
#10690 = CARTESIAN_POINT ( 'NONE',  ( -21.03221929538691271, 278.8698905765656377, -18.47759065022572855 ) ) ;
#10691 = CARTESIAN_POINT ( 'NONE',  ( 14.09825962131072785, 303.6587712403113528, 25.00000000000000000 ) ) ;
#10692 = CARTESIAN_POINT ( 'NONE',  ( -22.27502019258947286, 240.7448905683720000, -15.47720386886985544 ) ) ;
#10693 = CARTESIAN_POINT ( 'NONE',  ( -17.35679799567830273, 465.4323905765656946, 16.95518130045146421 ) ) ;
#10694 = SHAPE_REPRESENTATION ( 'Bronze Screw Shaft Nut Sleeve', ( #12794 ), #14893 ) ;
#10695 = CARTESIAN_POINT ( 'NONE',  ( -22.27502019258949062, 402.2448905683720568, -15.47720386886985544 ) ) ;
#10696 = DIRECTION ( 'NONE',  ( -1.000000000000000000, 0.000000000000000000, 0.000000000000000000 ) ) ;
#10697 = CARTESIAN_POINT ( 'NONE',  ( -28.68588794268871567, 354.7448905601784759, -19.99999999999999289 ) ) ;
#10698 = AXIS2_PLACEMENT_3D ( 'NONE', #9016, #4045, #7283 ) ;
#10699 = FACE_OUTER_BOUND ( 'NONE', #6908, .T. ) ;
#10700 = CARTESIAN_POINT ( 'NONE',  ( -22.27502019258949773, 460.7448905683720568, -15.47720386886985544 ) ) ;
#10701 = VERTEX_POINT ( 'NONE', #19578 ) ;
#10702 = CARTESIAN_POINT ( 'NONE',  ( -28.68588794268872277, 449.7448905601784759, 19.99999999999999289 ) ) ;
#10703 = ORIENTED_EDGE ( 'NONE', *, *, #5647, .F. ) ;
#10704 = DIRECTION ( 'NONE',  ( 0.000000000000000000, -1.000000000000000000, 0.000000000000000000 ) ) ;
#10705 = ORIENTED_EDGE ( 'NONE', *, *, #13688, .F. ) ;
#10706 = ORIENTED_EDGE ( 'NONE', *, *, #12926, .T. ) ;
#10707 = LINE ( 'NONE', #4237, #9056 ) ;
#10708 = CARTESIAN_POINT ( 'NONE',  ( -32.66413529028186957, 325.0573905601785327, -19.99999999999999289 ) ) ;
#10709 = CARTESIAN_POINT ( 'NONE',  ( -22.27502019258946930, 306.9948905683720568, 15.47720386886985189 ) ) ;
#10710 = CARTESIAN_POINT ( 'NONE',  ( -11.93348319268872260, 360.0573905683720000, 3.332260488124728859 ) ) ;
#10711 = CARTESIAN_POINT ( 'NONE',  ( -11.73070664223724080, 293.1823905601784759, -11.32908994701042538 ) ) ;
#10712 = VECTOR ( 'NONE', #17445, 1000.000000000000000 ) ;
#10713 = ADVANCED_FACE ( 'NONE', ( #4759 ), #11355, .T. ) ;
#10714 = CARTESIAN_POINT ( 'NONE',  ( -14.54375231895778775, 525.7448905765655809, 14.14213562373094568 ) ) ;
#10715 = CARTESIAN_POINT ( 'NONE',  ( -45.43829269268871229, 403.5573905683720000, -3.332260488124726194 ) ) ;
#10716 = CARTESIAN_POINT ( 'NONE',  ( -16.84014894278197616, 231.6198905683720000, -11.84573899990672707 ) ) ;
#10717 = CIRCLE ( 'NONE', #9354, 6.500000000000000888 ) ;
#10718 = CARTESIAN_POINT ( 'NONE',  ( -45.43829269268871940, 404.1823905683719431, 3.332260488124734632 ) ) ;
#10719 = CONTEXT_DEPENDENT_SHAPE_REPRESENTATION ( #1993, #9048 ) ;
#10720 = CARTESIAN_POINT ( 'NONE',  ( -48.68588794268870856, 351.9948905765656377, 0.000000000000000000 ) ) ;
#10721 = CYLINDRICAL_SURFACE ( 'NONE', #13106, 20.00000000000000000 ) ;
#10722 = CARTESIAN_POINT ( 'NONE',  ( -45.43829269268870519, 314.1823905683720000, 3.332260488124734632 ) ) ;
#10723 =( LENGTH_UNIT ( ) NAMED_UNIT ( * ) SI_UNIT ( .MILLI., .METRE. ) );
#10724 = VECTOR ( 'NONE', #4614, 1000.000000000000000 ) ;
#10725 = CARTESIAN_POINT ( 'NONE',  ( -38.17536295476246266, 456.9323905683720000, 14.20200298773971781 ) ) ;
#10727 = CARTESIAN_POINT ( 'NONE',  ( -48.68588794268873698, 573.2448905601785327, 0.000000000000000000 ) ) ;
#10726 = PRODUCT_DEFINITION_FORMATION_WITH_SPECIFIED_SOURCE ( 'ANY', '', #5764, .NOT_KNOWN. ) ;
#10728 = CARTESIAN_POINT ( 'NONE',  ( -14.31911992702480063, 585.7448905601785327, 19.70857778461545351 ) ) ;
#10729 = DIRECTION ( 'NONE',  ( -0.000000000000000000, -0.000000000000000000, -1.000000000000000000 ) ) ;
#10730 = VECTOR ( 'NONE', #20188, 1000.000000000000000 ) ;
#10731 = CARTESIAN_POINT ( 'NONE',  ( -44.16309181155856578, 365.9948905683720568, 6.410867750099241924 ) ) ;
#10732 = AXIS2_PLACEMENT_3D ( 'NONE', #15487, #673, #20237 ) ;
#10733 = CARTESIAN_POINT ( 'NONE',  ( 81.24038404635966515, 30.52886280891152282, -94.99999999999994316 ) ) ;
#10734 = CARTESIAN_POINT ( 'NONE',  ( -48.68588794268872277, 507.5573905601784759, 3.978247347593168115 ) ) ;
#10735 = CARTESIAN_POINT ( 'NONE',  ( -13.20868407381885667, 348.2448905683720000, 6.410867750099229490 ) ) ;
#10736 = EDGE_CURVE ( 'NONE', #20528, #20871, #8405, .T. ) ;
#10737 = ORIENTED_EDGE ( 'NONE', *, *, #219, .F. ) ;
#10738 = CARTESIAN_POINT ( 'NONE',  ( -14.48388495494901562, 507.9323905683720568, 9.489475012073732785 ) ) ;
#10739 = VECTOR ( 'NONE', #2255, 999.9999999999998863 ) ;
#10740 = DIRECTION ( 'NONE',  ( 0.000000000000000000, 1.000000000000000000, -0.000000000000000000 ) ) ;
#10741 = CARTESIAN_POINT ( 'NONE',  ( -22.27502019258948351, 418.4948905683720000, 15.47720386886985189 ) ) ;
#10742 = CARTESIAN_POINT ( 'NONE',  ( -14.54375231895776110, 288.2448905765656377, -14.14213562373094746 ) ) ;
#10743 = DIRECTION ( 'NONE',  ( 0.000000000000000000, 0.000000000000000000, -1.000000000000000000 ) ) ;
#10744 = CARTESIAN_POINT ( 'NONE',  ( -28.68588794268872988, 471.3698905683720568, -16.75240474999999307 ) ) ;
#10745 = EDGE_LOOP ( 'NONE', ( #20094, #13965 ) ) ;
#10746 = CARTESIAN_POINT ( 'NONE',  ( -38.17536295476246977, 462.3073905683720568, -14.20200298773971426 ) ) ;
#10747 = CARTESIAN_POINT ( 'NONE',  ( -45.43280446313950449, 223.9102039777116602, 0.4287796227366179602 ) ) ;
#10748 = CARTESIAN_POINT ( 'NONE',  ( -11.73070664223725146, 396.0573905765655809, 11.32908994701042005 ) ) ;
#10749 = CARTESIAN_POINT ( 'NONE',  ( 151.4788465195079823, 610.7448905601785327, -8.917803138848077182 ) ) ;
#10750 = AXIS2_PLACEMENT_3D ( 'NONE', #3677, #15160, #8753 ) ;
#10751 = CARTESIAN_POINT ( 'NONE',  ( -32.66413529028186957, 369.8073905765655240, -19.99999999999999289 ) ) ;
#10752 = CARTESIAN_POINT ( 'NONE',  ( 0.5805565836007611225, -3.752776749732563033, 6.500000000000000000 ) ) ;
#10753 = DIRECTION ( 'NONE',  ( -1.000000000000000000, -0.000000000000000000, -0.000000000000000000 ) ) ;
#10754 = ADVANCED_FACE ( 'NONE', ( #10161 ), #19742, .T. ) ;
#10755 = CARTESIAN_POINT ( 'NONE',  ( 4.700000000000000178, -3.752776749732563033, 6.500000000000000000 ) ) ;
#10756 = CARTESIAN_POINT ( 'NONE',  ( -47.16347859291443001, 237.8698905601784759, 7.653668647301805628 ) ) ;
#10757 = CARTESIAN_POINT ( 'NONE',  ( -42.82802356641964536, 205.1437886375728965, -5.000000000000001776 ) ) ;
#10758 = CARTESIAN_POINT ( 'NONE',  ( -38.17536295476244845, 273.8073905683720000, -14.20200298773971426 ) ) ;
#10759 = DIRECTION ( 'NONE',  ( -0.000000000000000000, -1.000000000000000000, -0.000000000000000000 ) ) ;
#10760 = CARTESIAN_POINT ( 'NONE',  ( -32.01814843081345430, 417.5573905683720568, 16.75240474999999307 ) ) ;
#10761 = CARTESIAN_POINT ( 'NONE',  ( -36.33955658999050797, 330.1198905765655809, -18.47759065022572855 ) ) ;
#10762 = CARTESIAN_POINT ( 'NONE',  ( -28.68588794268870146, 277.8698905683720000, 16.75240474999999307 ) ) ;
#10763 = ADVANCED_FACE ( 'NONE', ( #13746 ), #8536, .T. ) ;
#10764 = ORIENTED_EDGE ( 'NONE', *, *, #10939, .F. ) ;
#10765 = FACE_BOUND ( 'NONE', #20844, .T. ) ;
#10766 = EDGE_LOOP ( 'NONE', ( #6861, #13181, #5500, #2707 ) ) ;
#10767 = CARTESIAN_POINT ( 'NONE',  ( -42.88789093042844769, 474.4323905683721136, -9.489475012073734561 ) ) ;
#10768 = ORIENTED_EDGE ( 'NONE', *, *, #3976, .T. ) ;
#10769 = CARTESIAN_POINT ( 'NONE',  ( -21.03221929538692336, 364.1198905601785327, -18.47759065022572855 ) ) ;
#10770 = CARTESIAN_POINT ( 'NONE',  ( -11.93348319268870839, 239.1823905683720284, -3.332260488124732856 ) ) ;
#10771 = VERTEX_POINT ( 'NONE', #11895 ) ;
#10772 = CARTESIAN_POINT ( 'NONE',  ( -32.01814843081346140, 531.6823905683719431, -16.75240474999999307 ) ) ;
#10773 = CARTESIAN_POINT ( 'NONE',  ( -48.68588794268870856, 347.2448905601784759, 0.000000000000000000 ) ) ;
#10774 = CARTESIAN_POINT ( 'NONE',  ( -8.685887942688735208, 466.9948905765656377, -2.449293598294705724E-15 ) ) ;
#10775 = DIRECTION ( 'NONE',  ( 1.000000000000000000, 0.000000000000000000, 0.000000000000000000 ) ) ;
#10776 = DIRECTION ( 'NONE',  ( 0.000000000000000000, 0.000000000000000000, -1.000000000000000000 ) ) ;
#10777 = CARTESIAN_POINT ( 'NONE',  ( -25.77425622588650000, 223.9102039777116318, -18.75905995620974309 ) ) ;
#10778 = CARTESIAN_POINT ( 'NONE',  ( 0.000000000000000000, 0.000000000000000000, 0.000000000000000000 ) ) ;
#10779 = CARTESIAN_POINT ( 'NONE',  ( -11.93348319268873858, 510.0573905683720000, 3.332260488124728415 ) ) ;
#10780 = CARTESIAN_POINT ( 'NONE',  ( -48.68588794268872988, 517.2448905601785327, 0.000000000000000000 ) ) ;
#10781 = CARTESIAN_POINT ( 'NONE',  ( -13.20868407381884602, 238.2448905683720000, 6.410867750099229490 ) ) ;
#10782 = AXIS2_PLACEMENT_3D ( 'NONE', #14727, #19683, #4868 ) ;
#10783 = CARTESIAN_POINT ( 'NONE',  ( -19.19641293061498288, 341.9323905683720568, -14.20200298773971603 ) ) ;
#10784 = CARTESIAN_POINT ( 'NONE',  ( -21.03221929538692336, 470.3698905601784759, 18.47759065022572500 ) ) ;
#10785 = CARTESIAN_POINT ( 'NONE',  ( -42.82802356641965957, 358.4948905601785327, 14.14213562373094923 ) ) ;
#10786 = CARTESIAN_POINT ( 'NONE',  ( -38.17536295476246266, 392.3073905683720568, -14.20200298773971426 ) ) ;
#10787 = EDGE_CURVE ( 'NONE', #10157, #12627, #19053, .T. ) ;
#10788 = CIRCLE ( 'NONE', #16684, 20.57735571454641033 ) ;
#10789 = CARTESIAN_POINT ( 'NONE',  ( -36.33955658999051508, 389.1198905601784759, 18.47759065022572500 ) ) ;
#10790 = ADVANCED_FACE ( 'NONE', ( #15055 ), #346, .F. ) ;
#10791 = EDGE_LOOP ( 'NONE', ( #6963, #3249, #13535, #18158 ) ) ;
#10792 = DIRECTION ( 'NONE',  ( -1.191790137725560488E-16, 1.000000000000000000, 0.000000000000000000 ) ) ;
#10793 = VERTEX_POINT ( 'NONE', #8431 ) ;
#10794 = VERTEX_POINT ( 'NONE', #5503 ) ;
#10795 = CARTESIAN_POINT ( 'NONE',  ( -11.93348319268873858, 500.6823905683720568, -3.332260488124732856 ) ) ;
#10796 = CYLINDRICAL_SURFACE ( 'NONE', #11109, 19.99999999999999645 ) ;
#10797 = ORIENTED_EDGE ( 'NONE', *, *, #520, .T. ) ;
#10798 = CARTESIAN_POINT ( 'NONE',  ( -28.68588794268870856, 312.8698905683720000, -16.75240474999999307 ) ) ;
#10799 = PRODUCT_RELATED_PRODUCT_CATEGORY ( 'part', '', ( #5764 ) ) ;
#10800 = ORIENTED_EDGE ( 'NONE', *, *, #10876, .F. ) ;
#10801 = CARTESIAN_POINT ( 'NONE',  ( -11.93348319268872260, 338.5573905683720568, 3.332260488124728415 ) ) ;
#10802 = CARTESIAN_POINT ( 'NONE',  ( -40.53162694259543741, 342.6198905683720000, -11.84573899990672707 ) ) ;
#10803 = EDGE_CURVE ( 'NONE', #15800, #9575, #10473, .T. ) ;
#10804 = CARTESIAN_POINT ( 'NONE',  ( -17.35679799567828141, 275.4323905765656377, 16.95518130045146421 ) ) ;
#10805 = CARTESIAN_POINT ( 'NONE',  ( -18.81370552131602381, 585.7448905601785327, -6.112943483001347822 ) ) ;
#10806 = CARTESIAN_POINT ( 'NONE',  ( -19.19641293061496512, 247.3073905683720284, 14.20200298773971426 ) ) ;
#10807 = COLOUR_RGB ( '',0.7921568627450980005, 0.8196078431372548767, 0.9333333333333333481 ) ;
#10808 = CARTESIAN_POINT ( 'NONE',  ( -14.48388495494900496, 399.4323905683720568, 9.489475012073732785 ) ) ;
#10809 = EDGE_CURVE ( 'NONE', #15103, #17195, #19407, .T. ) ;
#10810 = DIRECTION ( 'NONE',  ( 0.000000000000000000, 1.000000000000000000, -0.000000000000000000 ) ) ;
#10811 = CARTESIAN_POINT ( 'NONE',  ( 4.700000000000000178, -3.752776749732576356, -6.499999999999999112 ) ) ;
#10812 = CARTESIAN_POINT ( 'NONE',  ( 2.416697501590669095, 172.9933428177121471, 50.00000000000000000 ) ) ;
#10813 = CARTESIAN_POINT ( 'NONE',  ( -38.17536295476246977, 452.3073905683720568, -14.20200298773971426 ) ) ;
#10814 = ORIENTED_EDGE ( 'NONE', *, *, #3669, .F. ) ;
#10815 = CARTESIAN_POINT ( 'NONE',  ( -40.01497788969913927, 438.8073905601784190, 16.95518130045146776 ) ) ;
#10816 = EDGE_CURVE ( 'NONE', #1524, #4442, #1442, .T. ) ;
#10817 = AXIS2_PLACEMENT_3D ( 'NONE', #18907, #13741, #2375 ) ;
#10818 = EDGE_LOOP ( 'NONE', ( #16132, #12214, #9990, #3771, #6758, #5713, #2932 ) ) ;
#10819 = CARTESIAN_POINT ( 'NONE',  ( -32.66413529028186957, 339.4323905601784190, 19.99999999999999289 ) ) ;
#10820 = ORIENTED_EDGE ( 'NONE', *, *, #577, .F. ) ;
#10821 = EDGE_LOOP ( 'NONE', ( #17924, #14307, #12277, #9072 ) ) ;
#10822 = CARTESIAN_POINT ( 'NONE',  ( 5.700000000000000178, 0.000000000000000000, 0.000000000000000000 ) ) ;
#10823 = CARTESIAN_POINT ( 'NONE',  ( -21.03221929538690560, 330.3698905601784759, 18.47759065022572500 ) ) ;
#10824 = AXIS2_PLACEMENT_3D ( 'NONE', #4908, #11504, #13356 ) ;
#10825 = CARTESIAN_POINT ( 'NONE',  ( -11.93348319268872260, 370.3698905683720568, -2.051577885510841163E-15 ) ) ;
#10826 = CARTESIAN_POINT ( 'NONE',  ( -45.64106924314016567, 228.1823905601784759, 11.32908994701042538 ) ) ;
#10827 = CARTESIAN_POINT ( 'NONE',  ( -48.68588794268872988, 531.9948905765656946, 0.000000000000000000 ) ) ;
#10828 = CARTESIAN_POINT ( 'NONE',  ( -14.48388495494900496, 409.8073905683720568, -9.489475012073736337 ) ) ;
#10829 = CARTESIAN_POINT ( 'NONE',  ( -40.53162694259542320, 246.6198905683720284, 11.84573899990672885 ) ) ;
#10830 = CARTESIAN_POINT ( 'NONE',  ( -16.84014894278199392, 400.1198905683720000, -11.84573899990672707 ) ) ;
#10831 = ITEM_DEFINED_TRANSFORMATION ( 'NONE', 'NONE', #16956,  #12794 ) ;
#10832 =( BOUNDED_CURVE ( )  B_SPLINE_CURVE ( 2, ( #2547, #5888, #6311, #19302, #16070, #11183, #12817, #10751, #938, #15859, #14240, #15751, #7505, #19408, #17464, #14349, #20714 ),
 .UNSPECIFIED., .F., .T. ) 
 B_SPLINE_CURVE_WITH_KNOTS ( ( 3, 2, 2, 2, 2, 2, 2, 2, 3 ),
 ( 0.5000000000000002220, 0.5019531250000002220, 0.5039062500000002220, 0.5058593750000002220, 0.5078125000000002220, 0.5097656250000002220, 0.5117187500000002220, 0.5136718750000002220, 0.5156250000000002220 ),
 .UNSPECIFIED. ) 
 CURVE ( )  GEOMETRIC_REPRESENTATION_ITEM ( )  RATIONAL_B_SPLINE_CURVE ( ( 0.9999999999999977796, 0.9807852804032326510, 1.000000000000000000, 0.9807852804032304306, 1.000000000000000000, 0.9807852804032304306, 1.000000000000000000, 0.9807852804032304306, 1.000000000000000000, 0.9807852804032304306, 1.000000000000000000, 0.9807852804032304306, 1.000000000000000000, 0.9807852804032304306, 1.000000000000000000, 0.9807852804032282101, 1.000000000000002220 ) ) 
 REPRESENTATION_ITEM ( '' )  );
#10833 = CARTESIAN_POINT ( 'NONE',  ( -10.20829729246298356, 337.6198905765656377, -7.653668647301794969 ) ) ;
#10834 = CARTESIAN_POINT ( 'NONE',  ( 88.28695088269886071, 152.5259582928263740, -40.00000000000000000 ) ) ;
#10835 = CARTESIAN_POINT ( 'NONE',  ( -16.84014894278197971, 307.6198905683720000, 11.84573899990672530 ) ) ;
#10836 =( NAMED_UNIT ( * ) SI_UNIT ( $, .STERADIAN. ) SOLID_ANGLE_UNIT ( ) );
#10837 = CARTESIAN_POINT ( 'NONE',  ( -45.43829269268871940, 455.0573905683720568, -3.332260488124726194 ) ) ;
#10838 = CARTESIAN_POINT ( 'NONE',  ( 5.074999999999999289, -3.752776749732561257, 6.500000000000000000 ) ) ;
#10839 = LINE ( 'NONE', #4355, #7614 ) ;
#10840 = DIRECTION ( 'NONE',  ( 0.000000000000000000, 0.000000000000000000, -1.000000000000000000 ) ) ;
#10841 = VECTOR ( 'NONE', #4411, 1000.000000000000000 ) ;
#10842 = CARTESIAN_POINT ( 'NONE',  ( -38.17536295476244845, 366.9323905683721136, 14.20200298773971781 ) ) ;
#10843 = CARTESIAN_POINT ( 'NONE',  ( -13.20868407381887621, 508.2448905683720568, 6.410867750099229490 ) ) ;
#10844 = EDGE_CURVE ( 'NONE', #10139, #11348, #4459, .T. ) ;
#10845 = CARTESIAN_POINT ( 'NONE',  ( -17.35679799567831338, 503.8073905601785327, -16.95518130045146421 ) ) ;
#10846 = CARTESIAN_POINT ( 'NONE',  ( -25.35362745456399125, 351.0573905683720568, -16.75240474999999307 ) ) ;
#10847 = VERTEX_POINT ( 'NONE', #17200 ) ;
#10848 = CARTESIAN_POINT ( 'NONE',  ( -25.35362745456400901, 511.0573905683720568, -16.75240474999999307 ) ) ;
#10849 = ORIENTED_EDGE ( 'NONE', *, *, #6033, .F. ) ;
#10850 = FACE_BOUND ( 'NONE', #11814, .T. ) ;
#10851 = CARTESIAN_POINT ( 'NONE',  ( -25.35362745456398770, 418.1823905683720568, 16.75240474999998952 ) ) ;
#10852 = CARTESIAN_POINT ( 'NONE',  ( -21.03221929538691626, 288.8698905765656377, -18.47759065022572855 ) ) ;
#10853 = CARTESIAN_POINT ( 'NONE',  ( -8.685887942688628627, 492.5573905601784190, -3.978247347592898553 ) ) ;
#10854 = CARTESIAN_POINT ( 'NONE',  ( -11.93348319268873503, 469.1823905683719431, -3.332260488124732856 ) ) ;
#10855 = ORIENTED_EDGE ( 'NONE', *, *, #19354, .F. ) ;
#10856 = CARTESIAN_POINT ( 'NONE',  ( -22.27502019258949062, 466.9948905683720000, 15.47720386886985189 ) ) ;
#10857 = CARTESIAN_POINT ( 'NONE',  ( -45.64106924314019409, 402.9323905765656946, 11.32908994701042715 ) ) ;
#10858 = CARTESIAN_POINT ( 'NONE',  ( 5.074999999999999289, 0.000000000000000000, 0.000000000000000000 ) ) ;
#10859 = DIRECTION ( 'NONE',  ( 1.000000000000000000, 0.000000000000000000, 0.000000000000000000 ) ) ;
#10860 = LINE ( 'NONE', #5889, #1168 ) ;
#10861 = DIRECTION ( 'NONE',  ( 0.000000000000000000, -1.000000000000000000, 0.000000000000000000 ) ) ;
#10862 = EDGE_CURVE ( 'NONE', #10281, #9782, #2810, .T. ) ;
#10863 = CARTESIAN_POINT ( 'NONE',  ( 158.8141120573112630, 610.7448905601785327, 0.000000000000000000 ) ) ;
#10864 = CARTESIAN_POINT ( 'NONE',  ( -42.82802356641964536, 238.4948905601784759, 14.14213562373094923 ) ) ;
#10865 = LINE ( 'NONE', #14354, #6934 ) ;
#10866 = CARTESIAN_POINT ( 'NONE',  ( -14.54375231895775578, 243.4948905601784759, -14.14213562373094746 ) ) ;
#10867 = LINE ( 'NONE', #12183, #5387 ) ;
#10868 = CARTESIAN_POINT ( 'NONE',  ( -25.35362745456399836, 432.5573905683719431, -16.75240474999999307 ) ) ;
#10869 = CARTESIAN_POINT ( 'NONE',  ( 60.03793209889851568, 30.52886280891152282, 131.1729372809869005 ) ) ;
#10870 = CARTESIAN_POINT ( 'NONE',  ( -38.17536295476243424, 256.9323905683720568, 14.20200298773971781 ) ) ;
#10871 = VERTEX_POINT ( 'NONE', #9394 ) ;
#10872 = ORIENTED_EDGE ( 'NONE', *, *, #3922, .T. ) ;
#10873 = CARTESIAN_POINT ( 'NONE',  ( 5.074999999999999289, 3.752776749732562589, 6.500000000000000000 ) ) ;
#10874 = ORIENTED_EDGE ( 'NONE', *, *, #10278, .F. ) ;
#10875 = CARTESIAN_POINT ( 'NONE',  ( -38.17536295476246977, 493.8073905683720000, -14.20200298773971426 ) ) ;
#10876 = EDGE_CURVE ( 'NONE', #6826, #12194, #6040, .T. ) ;
#10877 = EDGE_LOOP ( 'NONE', ( #9010, #2665, #12775, #8851 ) ) ;
#10878 = CARTESIAN_POINT ( 'NONE',  ( -8.685887942688742314, 526.9948905765655809, -2.449293598294705724E-15 ) ) ;
#10879 = CARTESIAN_POINT ( 'NONE',  ( -40.53162694259542320, 245.1198905683720284, 11.84573899990672885 ) ) ;
#10880 = ORIENTED_EDGE ( 'NONE', *, *, #7294, .T. ) ;
#10881 = CARTESIAN_POINT ( 'NONE',  ( -45.43829269268873361, 523.5573905683720568, -3.332260488124726638 ) ) ;
#10882 = DIRECTION ( 'NONE',  ( 0.5877852522924733591, 7.005166667827000450E-17, 0.8090169943749473402 ) ) ;
#10883 = FACE_OUTER_BOUND ( 'NONE', #3597, .T. ) ;
#10884 = DIRECTION ( 'NONE',  ( 1.000000000000000000, 0.000000000000000000, 0.000000000000000000 ) ) ;
#10885 = FACE_BOUND ( 'NONE', #11735, .T. ) ;
#10886 = CARTESIAN_POINT ( 'NONE',  ( -19.19641293061496867, 231.9323905683720000, -14.20200298773971603 ) ) ;
#10887 = EDGE_CURVE ( 'NONE', #10230, #14472, #9069, .T. ) ;
#10888 = CARTESIAN_POINT ( 'NONE',  ( -44.16309181155859420, 514.7448905683720568, -6.410867750099231266 ) ) ;
#10889 = CARTESIAN_POINT ( 'NONE',  ( -32.66413529028186957, 374.1823905765655809, 19.99999999999999289 ) ) ;
#10890 = CARTESIAN_POINT ( 'NONE',  ( -44.16309181155855867, 233.2448905683720000, -6.410867750099231266 ) ) ;
#10891 = CARTESIAN_POINT ( 'NONE',  ( -16.84014894278198682, 331.6198905683720000, -11.84573899990672707 ) ) ;
#10892 = DIRECTION ( 'NONE',  ( 0.000000000000000000, 0.000000000000000000, -1.000000000000000000 ) ) ;
#10893 = CARTESIAN_POINT ( 'NONE',  ( -11.73070664223723902, 306.0573905765655809, 11.32908994701042005 ) ) ;
#10894 = CARTESIAN_POINT ( 'NONE',  ( -22.27502019258947996, 376.9948905683720568, 15.47720386886985189 ) ) ;
#10895 = CARTESIAN_POINT ( 'NONE',  ( -8.685887942688895080, 326.6823905765656377, 3.978247347593586447 ) ) ;
#10896 = CARTESIAN_POINT ( 'NONE',  ( -11.73070664223725146, 383.1823905601784759, -11.32908994701042715 ) ) ;
#10897 = ORIENTED_EDGE ( 'NONE', *, *, #8477, .T. ) ;
#10898 = DIRECTION ( 'NONE',  ( 0.000000000000000000, 0.000000000000000000, 1.000000000000000000 ) ) ;
#10899 = EDGE_LOOP ( 'NONE', ( #8776, #19107, #18822 ) ) ;
#10900 = ORIENTED_EDGE ( 'NONE', *, *, #18151, .F. ) ;
#10901 = CARTESIAN_POINT ( 'NONE',  ( -11.93348319268873858, 510.3698905683720000, -2.051577885510841163E-15 ) ) ;
#10902 = CARTESIAN_POINT ( 'NONE',  ( -36.33955658999050797, 293.8698905765656377, 18.47759065022572500 ) ) ;
#10903 = VERTEX_POINT ( 'NONE', #2379 ) ;
#10904 = CARTESIAN_POINT ( 'NONE',  ( -16.84014894278198327, 311.6198905683720000, -11.84573899990672707 ) ) ;
#10905 = ORIENTED_EDGE ( 'NONE', *, *, #15971, .T. ) ;
#10906 = CARTESIAN_POINT ( 'NONE',  ( -28.68588794268871212, 331.3698905683720000, -16.75240474999999307 ) ) ;
#10907 = CARTESIAN_POINT ( 'NONE',  ( -13.20868407381885845, 349.4948905683720000, -6.410867750099233042 ) ) ;
#10908 = CARTESIAN_POINT ( 'NONE',  ( -21.03221929538691271, 268.8698905765656377, -18.47759065022572855 ) ) ;
#10909 = CARTESIAN_POINT ( 'NONE',  ( -10.20829729246298889, 392.8698905601784759, -7.653668647301794969 ) ) ;
#10910 = CARTESIAN_POINT ( 'NONE',  ( -38.17536295476243424, 245.4323905683720284, 14.20200298773971781 ) ) ;
#10911 = CARTESIAN_POINT ( 'NONE',  ( -45.43829269268871940, 405.3698905683720000, 0.000000000000000000 ) ) ;
#10912 = AXIS2_PLACEMENT_3D ( 'NONE', #254, #17862, #3380 ) ;
#10913 = CARTESIAN_POINT ( 'NONE',  ( -10.20829729246298179, 332.8698905601785327, -7.653668647301794969 ) ) ;
#10914 = FACE_OUTER_BOUND ( 'NONE', #14625, .T. ) ;
#10915 = CARTESIAN_POINT ( 'NONE',  ( -47.16347859291443001, 246.6198905601784759, -7.653668647301793193 ) ) ;
#10916 = VECTOR ( 'NONE', #9592, 1000.000000000000000 ) ;
#10917 = CARTESIAN_POINT ( 'NONE',  ( -45.43829269268871940, 443.8698905683720568, 0.000000000000000000 ) ) ;
#10918 = EDGE_LOOP ( 'NONE', ( #6013, #15229, #18613, #20284 ) ) ;
#10919 = CARTESIAN_POINT ( 'NONE',  ( -11.73070664223726034, 453.1823905601784759, -11.32908994701042715 ) ) ;
#10920 = EDGE_CURVE ( 'NONE', #4317, #339, #11781, .T. ) ;
#10921 = ORIENTED_EDGE ( 'NONE', *, *, #8030, .F. ) ;
#10922 = EDGE_LOOP ( 'NONE', ( #238, #4234, #20379, #3552 ) ) ;
#10923 = ORIENTED_EDGE ( 'NONE', *, *, #1759, .T. ) ;
#10924 = DIRECTION ( 'NONE',  ( 0.000000000000000000, -1.000000000000000000, 0.000000000000000000 ) ) ;
#10925 = CARTESIAN_POINT ( 'NONE',  ( -28.68588794268871212, 324.7448905601784759, -19.99999999999999289 ) ) ;
#10926 = EDGE_CURVE ( 'NONE', #19050, #7551, #7441, .T. ) ;
#10927 = ADVANCED_FACE ( 'NONE', ( #7660 ), #11009, .T. ) ;
#10928 = CARTESIAN_POINT ( 'NONE',  ( -11.93348319268872260, 370.0573905683719431, 3.332260488124728859 ) ) ;
#10929 = CARTESIAN_POINT ( 'NONE',  ( 35.96497763894178945, 230.5765313837437418, -60.00000000000000000 ) ) ;
#10930 = CARTESIAN_POINT ( 'NONE',  ( -45.64106924314020119, 501.0573905765656377, -11.32908994701042715 ) ) ;
#10931 = CARTESIAN_POINT ( 'NONE',  ( -45.43829269268870519, 383.5573905683720000, -3.332260488124726194 ) ) ;
#10932 = CARTESIAN_POINT ( 'NONE',  ( -45.43829269268869098, 245.0573905683720000, -3.332260488124726194 ) ) ;
#10933 = CARTESIAN_POINT ( 'NONE',  ( -13.20868407381886378, 398.2448905683720568, 6.410867750099229490 ) ) ;
#10934 = AXIS2_PLACEMENT_3D ( 'NONE', #4382, #4162, #12387 ) ;
#10935 = CARTESIAN_POINT ( 'NONE',  ( -17.35679799567828852, 335.4323905765656377, 16.95518130045146421 ) ) ;
#10936 = PLANE ( 'NONE',  #15521 ) ;
#10937 = CARTESIAN_POINT ( 'NONE',  ( -42.88789093042842637, 302.9323905683720568, -9.489475012073734561 ) ) ;
#10938 = CARTESIAN_POINT ( 'NONE',  ( -45.43829269268871940, 465.0573905683720000, -3.332260488124726194 ) ) ;
#10939 = EDGE_CURVE ( 'NONE', #10361, #2882, #12755, .T. ) ;
#10940 = CARTESIAN_POINT ( 'NONE',  ( 105.7989814974898479, 142.5259582928263455, 20.00000000000000355 ) ) ;
#10941 = CARTESIAN_POINT ( 'NONE',  ( -73.08746600497821078, 585.7448905601785327, 22.98912494155475628 ) ) ;
#10942 = CARTESIAN_POINT ( 'NONE',  ( 10.41669750159067220, 172.9933428177121471, -45.00000000000000000 ) ) ;
#10943 = AXIS2_PLACEMENT_3D ( 'NONE', #19091, #1351, #4275 ) ;
#10944 = CARTESIAN_POINT ( 'NONE',  ( -13.20868407381885845, 359.7448905683720568, 6.410867750099229490 ) ) ;
#10945 = CARTESIAN_POINT ( 'NONE',  ( -45.43829269268871940, 504.1823905683721136, 3.332260488124734632 ) ) ;
#10946 = CARTESIAN_POINT ( 'NONE',  ( -47.16347859291445843, 507.8698905601785327, 7.653668647301805628 ) ) ;
#10947 = CARTESIAN_POINT ( 'NONE',  ( -16.84014894278198327, 327.6198905683720000, 11.84573899990672530 ) ) ;
#10948 = VECTOR ( 'NONE', #1329, 1000.000000000000000 ) ;
#10949 = ORIENTED_EDGE ( 'NONE', *, *, #6691, .T. ) ;
#10950 = CARTESIAN_POINT ( 'NONE',  ( -32.01814843081346851, 506.0573905683719431, 16.75240474999999307 ) ) ;
#10951 = ORIENTED_EDGE ( 'NONE', *, *, #9134, .T. ) ;
#10952 =( BOUNDED_CURVE ( )  B_SPLINE_CURVE ( 2, ( #19151, #20447, #14295, #12229, #12654, #10586, #5620, #994, #9181, #667, #13860, #4103, #13974, #7340, #18812, #1099, #3993 ),
 .UNSPECIFIED., .F., .T. ) 
 B_SPLINE_CURVE_WITH_KNOTS ( ( 3, 2, 2, 2, 2, 2, 2, 2, 3 ),
 ( 0.09375000000000008327, 0.09570312500000011102, 0.09765625000000013878, 0.09960937500000016653, 0.1015625000000001943, 0.1035156250000002082, 0.1054687500000002359, 0.1074218750000002637, 0.1093750000000002914 ),
 .UNSPECIFIED. ) 
 CURVE ( )  GEOMETRIC_REPRESENTATION_ITEM ( )  RATIONAL_B_SPLINE_CURVE ( ( 0.9999999999999992228, 0.9807852804032312077, 1.000000000000000000, 0.9807852804032304306, 1.000000000000000000, 0.9807852804032304306, 1.000000000000000000, 0.9807852804032304306, 1.000000000000000000, 0.9807852804032304306, 1.000000000000000000, 0.9807852804032304306, 1.000000000000000000, 0.9807852804032304306, 1.000000000000000000, 0.9807852804032275440, 1.000000000000002887 ) ) 
 REPRESENTATION_ITEM ( '' )  );
#10953 = CARTESIAN_POINT ( 'NONE',  ( -28.68588794268870856, 314.4948905765656377, 19.99999999999999289 ) ) ;
#10954 = CARTESIAN_POINT ( 'NONE',  ( -11.93348319268872970, 430.3698905683720568, -2.051577885510841163E-15 ) ) ;
#10955 = CARTESIAN_POINT ( 'NONE',  ( -36.33955658999052218, 393.8698905765656377, 18.47759065022572500 ) ) ;
#10956 = FILL_AREA_STYLE_COLOUR ( '', #17295 ) ;
#10957 = CARTESIAN_POINT ( 'NONE',  ( -22.27502019258948707, 456.9948905683720000, 15.47720386886985189 ) ) ;
#10958 = VERTEX_POINT ( 'NONE', #15901 ) ;
#10959 = CARTESIAN_POINT ( 'NONE',  ( -38.17536295476246266, 465.4323905683720568, 14.20200298773971781 ) ) ;
#10960 = CARTESIAN_POINT ( 'NONE',  ( 0.000000000000000000, 0.000000000000000000, 0.000000000000000000 ) ) ;
#10961 = CARTESIAN_POINT ( 'NONE',  ( 79.78925230247502043, 142.5259582928263455, 20.00000000000000355 ) ) ;
#10962 = VECTOR ( 'NONE', #18653, 1000.000000000000000 ) ;
#10963 = CARTESIAN_POINT ( 'NONE',  ( -47.16347859291445133, 402.6198905765655809, 7.653668647301805628 ) ) ;
#10964 = CARTESIAN_POINT ( 'NONE',  ( 0.000000000000000000, 0.000000000000000000, 0.000000000000000000 ) ) ;
#10965 = CARTESIAN_POINT ( 'NONE',  ( -48.68588794268873698, 573.2448905601785327, 0.000000000000000000 ) ) ;
#10966 = DIRECTION ( 'NONE',  ( 1.000000000000000000, 0.000000000000000000, -0.000000000000000000 ) ) ;
#10967 = DIRECTION ( 'NONE',  ( 0.000000000000000000, 0.000000000000000000, 1.000000000000000000 ) ) ;
#10968 = CARTESIAN_POINT ( 'NONE',  ( 30.42502041961813575, 271.1055109169419097, -40.00000000000000000 ) ) ;
#10969 = CARTESIAN_POINT ( 'NONE',  ( -28.68588794268869435, 188.9102039777116602, 0.000000000000000000 ) ) ;
#10970 = CARTESIAN_POINT ( 'NONE',  ( -44.28481028704773337, 223.9102039777117454, 9.367795489887496885 ) ) ;
#10971 = CARTESIAN_POINT ( 'NONE',  ( -24.70764059509553334, 240.0573905601784759, 19.99999999999998934 ) ) ;
#10972 = CARTESIAN_POINT ( 'NONE',  ( -21.03221929538691981, 450.3698905601784759, 18.47759065022572500 ) ) ;
#10973 = CARTESIAN_POINT ( 'NONE',  ( -11.93348319268872970, 430.3698905683720568, -2.051577885510841163E-15 ) ) ;
#10974 = CARTESIAN_POINT ( 'NONE',  ( -42.82802356641965957, 385.9948905601784759, -14.14213562373094746 ) ) ;
#10975 = CARTESIAN_POINT ( 'NONE',  ( -11.93348319268870839, 250.0573905683720000, 3.332260488124728415 ) ) ;
#10976 = EDGE_LOOP ( 'NONE', ( #5928, #6158, #4974, #7219 ) ) ;
#10977 = ORIENTED_EDGE ( 'NONE', *, *, #13147, .T. ) ;
#10978 = CARTESIAN_POINT ( 'NONE',  ( -19.19641293061499354, 461.9323905683720568, -14.20200298773971603 ) ) ;
#10979 = CARTESIAN_POINT ( 'NONE',  ( -48.68588794268869435, 231.9948905765656377, 0.000000000000000000 ) ) ;
#10980 = ADVANCED_FACE ( 'NONE', ( #14288 ), #10796, .T. ) ;
#10981 = ORIENTED_EDGE ( 'NONE', *, *, #8300, .T. ) ;
#10982 = DIRECTION ( 'NONE',  ( -1.191790137725560488E-16, 1.000000000000000000, -0.000000000000000000 ) ) ;
#10983 = CARTESIAN_POINT ( 'NONE',  ( -16.84014894278197616, 240.1198905683720284, -11.84573899990672707 ) ) ;
#10984 = ORIENTED_EDGE ( 'NONE', *, *, #14317, .F. ) ;
#10985 = CARTESIAN_POINT ( 'NONE',  ( -28.68588794268872988, 516.3698905683720568, 16.75240474999999307 ) ) ;
#10986 = CARTESIAN_POINT ( 'NONE',  ( -31.26501780185373391, 205.1437886375728965, -5.000000000000001776 ) ) ;
#10987 = CARTESIAN_POINT ( 'NONE',  ( -48.68588794268872277, 461.9948905765656377, 0.000000000000000000 ) ) ;
#10988 = CARTESIAN_POINT ( 'NONE',  ( -45.64106924314017988, 348.1823905601784759, 11.32908994701042538 ) ) ;
#10989 = ADVANCED_FACE ( 'NONE', ( #16013 ), #8961, .F. ) ;
#10990 = CARTESIAN_POINT ( 'NONE',  ( -48.68588794268879383, 282.3073905765656946, 3.978247347592954952 ) ) ;
#10991 = CARTESIAN_POINT ( 'NONE',  ( -24.85637767767141426, 223.9102039777116033, -18.72850036933187212 ) ) ;
#10992 = DIRECTION ( 'NONE',  ( 0.000000000000000000, -1.000000000000000000, 0.000000000000000000 ) ) ;
#10993 = VECTOR ( 'NONE', #18785, 1000.000000000000000 ) ;
#10994 = DIRECTION ( 'NONE',  ( 0.000000000000000000, 1.000000000000000000, 0.000000000000000000 ) ) ;
#10995 = CARTESIAN_POINT ( 'NONE',  ( -22.27502019258947286, 230.7448905683720000, -15.47720386886985544 ) ) ;
#10996 = CARTESIAN_POINT ( 'NONE',  ( -19.19641293061497933, 328.8073905683720568, 14.20200298773971426 ) ) ;
#10997 = CARTESIAN_POINT ( 'NONE',  ( -48.68588794268887199, 317.5573905601785327, 3.978247347592742678 ) ) ;
#10998 = DIRECTION ( 'NONE',  ( 0.000000000000000000, 0.000000000000000000, -1.000000000000000000 ) ) ;
#10999 = CARTESIAN_POINT ( 'NONE',  ( -28.68588794268870856, 302.8698905683720000, -16.75240474999999307 ) ) ;
#11000 = CARTESIAN_POINT ( 'NONE',  ( -40.53162694259543741, 382.6198905683720568, -11.84573899990672707 ) ) ;
#11001 = CARTESIAN_POINT ( 'NONE',  ( -22.27502019258949773, 528.4948905683719431, 15.47720386886985189 ) ) ;
#11002 = CARTESIAN_POINT ( 'NONE',  ( -40.01497788969914637, 395.6823905601784190, -16.95518130045146421 ) ) ;
#11003 = VECTOR ( 'NONE', #20826, 1000.000000000000000 ) ;
#11004 = EDGE_CURVE ( 'NONE', #12520, #12450, #3521, .T. ) ;
#11005 = FACE_OUTER_BOUND ( 'NONE', #12495, .T. ) ;
#11006 = ORIENTED_EDGE ( 'NONE', *, *, #3281, .F. ) ;
#11007 = EDGE_LOOP ( 'NONE', ( #2331, #5477, #1694, #7594, #3624, #10417 ) ) ;
#11008 = CARTESIAN_POINT ( 'NONE',  ( -38.17536295476247687, 513.8073905683720568, -14.20200298773971426 ) ) ;
#11009 = PLANE ( 'NONE',  #4200 ) ;
#11010 = B_SPLINE_CURVE_WITH_KNOTS ( 'NONE', 3,
 ( #17314, #7450, #8763, #8650, #18921, #5405, #15700, #18602, #13976, #7027, #562, #15383, #10272, #13649, #886, #5622, #15596, #4105, #20558, #2073, #20234, #12116 ),
 .UNSPECIFIED., .F., .F.,
 ( 4, 2, 2, 2, 2, 2, 2, 2, 2, 2, 4 ),
 ( 0.02361608169583585826, 0.02460001686704672841, 0.02509198445265212185, 0.02558395203825751876, 0.02656788720946830565, 0.02755182238067909600, 0.02853575755188988289, 0.02951969272310067324, 0.03001166030870608403, 0.03050362789431149482, 0.03148756306552229906 ),
 .UNSPECIFIED. ) ;
#11011 = ORIENTED_EDGE ( 'NONE', *, *, #15553, .F. ) ;
#11012 = CARTESIAN_POINT ( 'NONE',  ( -44.16309181155855867, 295.9948905683720000, 6.410867750099241924 ) ) ;
#11013 = CARTESIAN_POINT ( 'NONE',  ( -14.48388495494899608, 329.8073905683720000, -9.489475012073736337 ) ) ;
#11014 = CARTESIAN_POINT ( 'NONE',  ( -48.68588794268870146, 271.9948905765656377, 0.000000000000000000 ) ) ;
#11015 = CARTESIAN_POINT ( 'NONE',  ( -11.73070664223725323, 393.1823905601785896, -11.32908994701042538 ) ) ;
#11016 = CARTESIAN_POINT ( 'NONE',  ( -45.43829269268869808, 243.5573905683720000, -3.332260488124726638 ) ) ;
#11017 = CARTESIAN_POINT ( 'NONE',  ( -11.93348319268872615, 400.3698905683720000, -2.051577885510841163E-15 ) ) ;
#11018 = AXIS2_PLACEMENT_3D ( 'NONE', #13328, #8648, #458 ) ;
#11019 = EDGE_CURVE ( 'NONE', #13344, #5669, #9039, .T. ) ;
#11020 = CARTESIAN_POINT ( 'NONE',  ( -28.68588794268873698, 548.2448905601784190, 0.000000000000000000 ) ) ;
#11021 = CARTESIAN_POINT ( 'NONE',  ( 5.074999999999999289, 7.511572993685795156E-16, -6.500000000000000000 ) ) ;
#11022 = CARTESIAN_POINT ( 'NONE',  ( -17.35679799567831338, 508.5573905765655809, -16.95518130045146421 ) ) ;
#11023 = CARTESIAN_POINT ( 'NONE',  ( -22.27502019258948707, 446.9948905683720000, 15.47720386886985189 ) ) ;
#11024 = ORIENTED_EDGE ( 'NONE', *, *, #3136, .F. ) ;
#11025 = CARTESIAN_POINT ( 'NONE',  ( -21.03221929538693402, 454.1198905601784759, -18.47759065022572855 ) ) ;
#11026 = ADVANCED_FACE ( 'NONE', ( #17412 ), #4532, .T. ) ;
#11027 = VERTEX_POINT ( 'NONE', #7333 ) ;
#11028 = ORIENTED_EDGE ( 'NONE', *, *, #13469, .F. ) ;
#11029 = ORIENTED_EDGE ( 'NONE', *, *, #20952, .F. ) ;
#11030 = CARTESIAN_POINT ( 'NONE',  ( 3.458603197740078627, 230.5765313837437418, 33.59072564020503648 ) ) ;
#11031 = CARTESIAN_POINT ( 'NONE',  ( -24.70764059509555821, 324.4323905601784190, -19.99999999999999289 ) ) ;
#11032 = CARTESIAN_POINT ( 'NONE',  ( -11.06088464903280233, 326.0737056351150613, 5.773301668816269938 ) ) ;
#11033 = CONICAL_SURFACE ( 'NONE', #2768, 6.500000000000000000, 1.047197551196600296 ) ;
#11034 = CARTESIAN_POINT ( 'NONE',  ( -14.48388495494899786, 359.4323905683720000, 9.489475012073731008 ) ) ;
#11035 = CARTESIAN_POINT ( 'NONE',  ( -28.68588794268874054, 573.2448905601785327, 0.000000000000000000 ) ) ;
#11036 = CARTESIAN_POINT ( 'NONE',  ( -24.70764059509557953, 509.1823905765655240, -19.99999999999999289 ) ) ;
#11037 = CARTESIAN_POINT ( 'NONE',  ( -32.01814843081344719, 386.0573905683720000, 16.75240474999999307 ) ) ;
#11038 = CARTESIAN_POINT ( 'NONE',  ( -44.16309181155855867, 224.7448905683720568, -6.410867750099231266 ) ) ;
#11039 = CARTESIAN_POINT ( 'NONE',  ( -11.93348319268872615, 409.1823905683720568, -3.332260488124732856 ) ) ;
#11040 = CARTESIAN_POINT ( 'NONE',  ( -28.68588794268871212, 329.4948905765656377, -19.99999999999999289 ) ) ;
#11041 = CARTESIAN_POINT ( 'NONE',  ( 6.416697501590670427, 217.7548513357008630, 60.00000000000000000 ) ) ;
#11042 = CARTESIAN_POINT ( 'NONE',  ( -35.09675569278794427, 305.7448905683720568, 15.47720386886985366 ) ) ;
#11043 = SHAPE_REPRESENTATION_RELATIONSHIP ( 'NONE' , 'NONE' ,  #15840, #2751 ) ;
#11044 = CARTESIAN_POINT ( 'NONE',  ( -19.19641293061498999, 448.8073905683720568, 14.20200298773971426 ) ) ;
#11045 = DIRECTION ( 'NONE',  ( 2.775557561562891844E-16, 0.000000000000000000, 1.000000000000000000 ) ) ;
#11046 = CARTESIAN_POINT ( 'NONE',  ( -10.20829729246298712, 371.6198905601784759, 7.653668647301790529 ) ) ;
#11047 = DIRECTION ( 'NONE',  ( 0.000000000000000000, -1.000000000000000000, 0.000000000000000000 ) ) ;
#11048 = CARTESIAN_POINT ( 'NONE',  ( -32.01814843081344719, 373.1823905683720000, -16.75240474999999307 ) ) ;
#11049 = CARTESIAN_POINT ( 'NONE',  ( -19.19641293061500065, 510.4323905683720000, -14.20200298773971603 ) ) ;
#11050 = CARTESIAN_POINT ( 'NONE',  ( -8.685887942688740537, 501.9323905601784759, 3.978247347593161010 ) ) ;
#11051 = CARTESIAN_POINT ( 'NONE',  ( -40.53162694259543031, 322.6198905683720568, -11.84573899990672707 ) ) ;
#11052 = ORIENTED_EDGE ( 'NONE', *, *, #492, .T. ) ;
#11053 = VECTOR ( 'NONE', #744, 1000.000000000000114 ) ;
#11054 = CARTESIAN_POINT ( 'NONE',  ( -46.31968306282883674, 135.1716627696692683, 33.59072564020503648 ) ) ;
#11055 = VERTEX_POINT ( 'NONE', #13964 ) ;
#11056 = CLOSED_SHELL ( 'NONE', ( #4384, #14787, #13721, #7711, #18595, #20159, #16773, #8738, #12137, #18044, #17390, #6899, #11598, #8547, #12537, #1799, #3352, #7428, #10267 ) ) ;
#11057 = ADVANCED_FACE ( 'NONE', ( #12861 ), #11437, .F. ) ;
#11058 = CARTESIAN_POINT ( 'NONE',  ( -41.83569717483972994, 213.9102039777116602, 24.99999999999998579 ) ) ;
#11059 = ADVANCED_FACE ( 'NONE', ( #5056 ), #19451, .T. ) ;
#11060 = CARTESIAN_POINT ( 'NONE',  ( -32.01814843081344719, 417.5573905683720568, 16.75240474999999307 ) ) ;
#11061 = CARTESIAN_POINT ( 'NONE',  ( -45.64106924314018698, 392.9323905765655809, 11.32908994701042538 ) ) ;
#11062 = DIRECTION ( 'NONE',  ( 0.000000000000000000, 1.000000000000000000, -0.000000000000000000 ) ) ;
#11063 = CARTESIAN_POINT ( 'NONE',  ( -25.35362745456399125, 436.6823905683720000, 16.75240474999998952 ) ) ;
#11064 = ORIENTED_EDGE ( 'NONE', *, *, #2565, .F. ) ;
#11065 = CARTESIAN_POINT ( 'NONE',  ( -14.48388495494901029, 459.8073905683720000, -9.489475012073734561 ) ) ;
#11066 = CARTESIAN_POINT ( 'NONE',  ( 0.000000000000000000, 0.000000000000000000, 0.000000000000000000 ) ) ;
#11067 = PLANE ( 'NONE',  #20706 ) ;
#11068 = PRODUCT_DEFINITION_FORMATION_WITH_SPECIFIED_SOURCE ( 'ANY', '', #19604, .NOT_KNOWN. ) ;
#11069 = CARTESIAN_POINT ( 'NONE',  ( -42.82802356641966668, 393.2448905765655809, 14.14213562373094923 ) ) ;
#11070 = CARTESIAN_POINT ( 'NONE',  ( -8.685887942688712116, 276.9948905765656377, -2.449293598294705724E-15 ) ) ;
#11071 = PRODUCT_DEFINITION ( 'UNKNOWN', '', #15246, #3586 ) ;
#11072 = DIRECTION ( 'NONE',  ( 0.000000000000000000, 1.000000000000000000, -0.000000000000000000 ) ) ;
#11073 = CARTESIAN_POINT ( 'NONE',  ( -28.68588794268872633, 271.1055109169419666, -40.00000000000000000 ) ) ;
#11074 = DIRECTION ( 'NONE',  ( 1.191790137725560488E-16, -1.000000000000000000, -0.000000000000000000 ) ) ;
#11075 = AXIS2_PLACEMENT_3D ( 'NONE', #6513, #6404, #1141 ) ;
#11076 = CARTESIAN_POINT ( 'NONE',  ( 69.79185940953689737, 142.2976266388001250, 40.00000000000000000 ) ) ;
#11077 = VECTOR ( 'NONE', #7775, 1000.000000000000000 ) ;
#11078 = CARTESIAN_POINT ( 'NONE',  ( -24.70764059509554755, 254.4323905601784759, -19.99999999999999289 ) ) ;
#11079 = CARTESIAN_POINT ( 'NONE',  ( -43.68588794268869435, 213.9102039777116602, 0.000000000000000000 ) ) ;
#11080 = CARTESIAN_POINT ( 'NONE',  ( -16.84014894278199392, 419.1198905683720000, 11.84573899990672530 ) ) ;
#11081 = DIRECTION ( 'NONE',  ( -1.191790137725560488E-16, 1.000000000000000000, -0.000000000000000000 ) ) ;
#11082 = AXIS2_PLACEMENT_3D ( 'NONE', #3553, #5482, #6997 ) ;
#11083 =( BOUNDED_CURVE ( )  B_SPLINE_CURVE ( 2, ( #6775, #2038, #18355, #16645, #2249, #11653, #11867, #15444, #208, #15346, #10020, #8607, #13396, #20305, #5475, #1829, #3855 ),
 .UNSPECIFIED., .F., .T. ) 
 B_SPLINE_CURVE_WITH_KNOTS ( ( 3, 2, 2, 2, 2, 2, 2, 2, 3 ),
 ( 0.000000000000000000, 0.001953125000000046838, 0.003906250000000093675, 0.005859375000000140513, 0.007812500000000187350, 0.009765625000000234188, 0.01171875000000028103, 0.01367187500000032786, 0.01562500000000037470 ),
 .UNSPECIFIED. ) 
 CURVE ( )  GEOMETRIC_REPRESENTATION_ITEM ( )  RATIONAL_B_SPLINE_CURVE ( ( 1.000000000000000000, 0.9807852804032304306, 1.000000000000000000, 0.9807852804032304306, 1.000000000000000000, 0.9807852804032304306, 1.000000000000000000, 0.9807852804032304306, 1.000000000000000000, 0.9807852804032304306, 1.000000000000000000, 0.9807852804032304306, 1.000000000000000000, 0.9807852804032304306, 1.000000000000000000, 0.9807852804032267668, 1.000000000000003775 ) ) 
 REPRESENTATION_ITEM ( '' )  );
#11084 = CARTESIAN_POINT ( 'NONE',  ( -35.09675569278793006, 243.4948905683720284, -15.47720386886985544 ) ) ;
#11085 = VERTEX_POINT ( 'NONE', #3123 ) ;
#11086 = EDGE_LOOP ( 'NONE', ( #19079, #5363, #18402, #11762 ) ) ;
#11087 = DIRECTION ( 'NONE',  ( -1.191790137725560488E-16, 1.000000000000000000, -0.000000000000000000 ) ) ;
#11088 = ORIENTED_EDGE ( 'NONE', *, *, #14673, .T. ) ;
#11089 = CARTESIAN_POINT ( 'NONE',  ( -28.68588794268872633, 467.8698905683720000, 16.75240474999999307 ) ) ;
#11090 = CARTESIAN_POINT ( 'NONE',  ( -40.01497788969911795, 223.5573905765656093, 16.95518130045146776 ) ) ;
#11091 = VECTOR ( 'NONE', #18275, 1000.000000000000000 ) ;
#11092 = ORIENTED_EDGE ( 'NONE', *, *, #17674, .F. ) ;
#11093 = CARTESIAN_POINT ( 'NONE',  ( 107.6674317086782935, 187.4856410316723441, -20.00000000000000355 ) ) ;
#11094 = CARTESIAN_POINT ( 'NONE',  ( -35.09675569278793716, 225.7448905683720568, 15.47720386886985366 ) ) ;
#11095 =( REPRESENTATION_RELATIONSHIP ('NONE','NONE', #1888, #7793 ) REPRESENTATION_RELATIONSHIP_WITH_TRANSFORMATION ( #17129 )SHAPE_REPRESENTATION_RELATIONSHIP( ) );
#11096 = ORIENTED_EDGE ( 'NONE', *, *, #7575, .F. ) ;
#11097 = CARTESIAN_POINT ( 'NONE',  ( -16.84014894278200813, 527.6198905683719431, 11.84573899990672530 ) ) ;
#11098 = LINE ( 'NONE', #13159, #10724 ) ;
#11099 = CARTESIAN_POINT ( 'NONE',  ( -21.03221929538691981, 455.1198905765655809, 18.47759065022572500 ) ) ;
#11100 = FACE_OUTER_BOUND ( 'NONE', #6881, .T. ) ;
#11101 = DIRECTION ( 'NONE',  ( -0.000000000000000000, -1.000000000000000000, -0.000000000000000000 ) ) ;
#11102 = DIRECTION ( 'NONE',  ( -1.191790137725560488E-16, 1.000000000000000000, -0.000000000000000000 ) ) ;
#11103 = DIRECTION ( 'NONE',  ( 1.000000000000000000, 0.000000000000000000, 0.000000000000000000 ) ) ;
#11104 = SURFACE_STYLE_USAGE ( .BOTH. , #12953 ) ;
#11105 = CARTESIAN_POINT ( 'NONE',  ( -35.09675569278793006, 231.9948905683720284, -15.47720386886985544 ) ) ;
#11106 = CARTESIAN_POINT ( 'NONE',  ( -40.53162694259543031, 324.1198905683720568, -11.84573899990672707 ) ) ;
#11107 = CARTESIAN_POINT ( 'NONE',  ( -21.03221929538693402, 444.1198905601784759, -18.47759065022572855 ) ) ;
#11108 = CARTESIAN_POINT ( 'NONE',  ( -11.73070664223724791, 381.3073905601784759, 11.32908994701042005 ) ) ;
#11109 = AXIS2_PLACEMENT_3D ( 'NONE', #12432, #20874, #17619 ) ;
#11110 = CARTESIAN_POINT ( 'NONE',  ( -44.16309181155855867, 315.9948905683720568, 6.410867750099241924 ) ) ;
#11111 = CARTESIAN_POINT ( 'NONE',  ( -38.17536295476244845, 385.4323905683720000, 14.20200298773971781 ) ) ;
#11112 = ADVANCED_FACE ( 'NONE', ( #21076 ), #16327, .T. ) ;
#11113 = CARTESIAN_POINT ( 'NONE',  ( -14.48388495494901917, 531.3073905683719431, -9.489475012073734561 ) ) ;
#11114 = CARTESIAN_POINT ( 'NONE',  ( -8.685887942688720997, 362.5573905601784759, -3.978247347593165895 ) ) ;
#11115 = CARTESIAN_POINT ( 'NONE',  ( -28.68588794268870146, 229.4948905765656377, -19.99999999999999289 ) ) ;
#11116 = ORIENTED_EDGE ( 'NONE', *, *, #18647, .F. ) ;
#11117 = CARTESIAN_POINT ( 'NONE',  ( -16.84014894278200458, 491.6198905683720000, -11.84573899990672707 ) ) ;
#11118 = DIRECTION ( 'NONE',  ( -1.000000000000000000, 0.000000000000000000, 0.000000000000000000 ) ) ;
#11119 = CARTESIAN_POINT ( 'NONE',  ( -19.19641293061497578, 307.3073905683720000, 14.20200298773971426 ) ) ;
#11120 = ORIENTED_EDGE ( 'NONE', *, *, #10224, .F. ) ;
#11121 = CARTESIAN_POINT ( 'NONE',  ( -11.93348319268871194, 290.3698905683720568, -2.051577885510841163E-15 ) ) ;
#11122 = CARTESIAN_POINT ( 'NONE',  ( -45.43829269268870519, 323.8698905683720000, 0.000000000000000000 ) ) ;
#11123 = AXIS2_PLACEMENT_3D ( 'NONE', #15434, #518, #12504 ) ;
#11124 = CARTESIAN_POINT ( 'NONE',  ( -42.82802356641965247, 273.2448905765656377, 14.14213562373094923 ) ) ;
#11125 = LINE ( 'NONE', #9609, #3 ) ;
#11126 = CARTESIAN_POINT ( 'NONE',  ( -28.68588794268870146, 231.3698905683720284, -16.75240474999999307 ) ) ;
#11127 = CARTESIAN_POINT ( 'NONE',  ( -25.35362745456398414, 378.1823905683720568, 16.75240474999998952 ) ) ;
#11128 = EDGE_CURVE ( 'NONE', #11298, #8982, #1503, .T. ) ;
#11129 = LINE ( 'NONE', #1407, #20984 ) ;
#11130 = CARTESIAN_POINT ( 'NONE',  ( -48.68588794268869435, 257.2448905601784759, 0.000000000000000000 ) ) ;
#11131 = PRODUCT_DEFINITION_SHAPE ( 'NONE', 'NONE',  #21398 ) ;
#11132 = B_SPLINE_CURVE_WITH_KNOTS ( 'NONE', 3,
 ( #5372, #7101, #19882, #19991, #10453, #20103, #5171, #15033 ),
 .UNSPECIFIED., .F., .F.,
 ( 4, 2, 2, 4 ),
 ( 0.003797433802554430696, 0.004743183970586230085, 0.005688934138618029039, 0.007580434474681626081 ),
 .UNSPECIFIED. ) ;
#11133 = AXIS2_PLACEMENT_3D ( 'NONE', #2445, #12386, #9026 ) ;
#11134 = CARTESIAN_POINT ( 'NONE',  ( -47.16347859291446554, 511.3698905765655809, -7.653668647301793193 ) ) ;
#11135 = CARTESIAN_POINT ( 'NONE',  ( -13.20868407381887089, 439.4948905683720568, -6.410867750099233042 ) ) ;
#11136 = CARTESIAN_POINT ( 'NONE',  ( 5.074999999999999289, -3.752776749732576356, -6.500000000000000000 ) ) ;
#11137 = EDGE_LOOP ( 'NONE', ( #12448, #20076, #14192, #6427 ) ) ;
#11138 = CARTESIAN_POINT ( 'NONE',  ( -42.82802356641966668, 448.4948905601784759, 14.14213562373094923 ) ) ;
#11139 = ORIENTED_EDGE ( 'NONE', *, *, #20021, .T. ) ;
#11140 = ORIENTED_EDGE ( 'NONE', *, *, #15849, .T. ) ;
#11141 = LINE ( 'NONE', #12985, #8009 ) ;
#11142 = CARTESIAN_POINT ( 'NONE',  ( -42.82802356641965957, 335.9948905601784759, -14.14213562373094746 ) ) ;
#11143 = CARTESIAN_POINT ( 'NONE',  ( -45.43280446313950449, 223.9102039777116602, 0.4287796227366179602 ) ) ;
#11144 = EDGE_CURVE ( 'NONE', #13614, #13852, #18037, .T. ) ;
#11145 = CARTESIAN_POINT ( 'NONE',  ( -16.84014894278199037, 371.6198905683720000, -11.84573899990672707 ) ) ;
#11146 = CARTESIAN_POINT ( 'NONE',  ( -48.68588794268873698, 573.2448905601785327, 0.000000000000000000 ) ) ;
#11147 = CARTESIAN_POINT ( 'NONE',  ( -21.03221929538692692, 495.1198905765656377, 18.47759065022572500 ) ) ;
#11148 = CARTESIAN_POINT ( 'NONE',  ( -42.88789093042844058, 392.9323905683720568, -9.489475012073736337 ) ) ;
#11149 = CARTESIAN_POINT ( 'NONE',  ( -28.68588794268869790, 222.8698905683720284, -16.75240474999999307 ) ) ;
#11150 = VECTOR ( 'NONE', #19433, 1000.000000000000114 ) ;
#11151 = CARTESIAN_POINT ( 'NONE',  ( -35.09675569278795138, 391.9948905683720568, -15.47720386886985544 ) ) ;
#11152 = MANIFOLD_SOLID_BREP ( 'Cut-Extrude9', #728 ) ;
#11153 = CARTESIAN_POINT ( 'NONE',  ( -36.33955658999050087, 320.1198905765656377, -18.47759065022572855 ) ) ;
#11154 = CARTESIAN_POINT ( 'NONE',  ( 60.03793209889851568, 30.52886280891152282, 136.1729372809869005 ) ) ;
#11155 = CARTESIAN_POINT ( 'NONE',  ( -25.35362745456398059, 281.0573905683720568, -16.75240474999999307 ) ) ;
#11156 = CARTESIAN_POINT ( 'NONE',  ( -35.09675569278796559, 467.2448905683720568, 15.47720386886985366 ) ) ;
#11157 = EDGE_CURVE ( 'NONE', #15737, #8903, #6609, .T. ) ;
#11158 = DIRECTION ( 'NONE',  ( 0.000000000000000000, 0.000000000000000000, -1.000000000000000000 ) ) ;
#11159 = CARTESIAN_POINT ( 'NONE',  ( -48.68588794268871567, 417.2448905601784759, 0.000000000000000000 ) ) ;
#11160 = LINE ( 'NONE', #7589, #14058 ) ;
#11161 = VECTOR ( 'NONE', #3252, 1000.000000000000000 ) ;
#11162 = CARTESIAN_POINT ( 'NONE',  ( -40.53162694259543741, 376.6198905683720568, 11.84573899990672885 ) ) ;
#11163 = CARTESIAN_POINT ( 'NONE',  ( -42.88789093042845479, 512.9323905683719431, -9.489475012073736337 ) ) ;
#11164 = AXIS2_PLACEMENT_3D ( 'NONE', #5998, #10966, #2766 ) ;
#11165 = CARTESIAN_POINT ( 'NONE',  ( -11.73070664223726745, 513.1823905601785327, -11.32908994701042715 ) ) ;
#11166 = CARTESIAN_POINT ( 'NONE',  ( -44.16309181155855867, 324.4948905683720568, 6.410867750099241924 ) ) ;
#11167 = VERTEX_POINT ( 'NONE', #6250 ) ;
#11168 = CARTESIAN_POINT ( 'NONE',  ( -17.35679799567831694, 523.8073905601784190, -16.95518130045146421 ) ) ;
#11169 = EDGE_LOOP ( 'NONE', ( #9964, #7462, #12268, #5419 ) ) ;
#11170 = CARTESIAN_POINT ( 'NONE',  ( -33.23992160639906501, 53.12908672755433770, 49.39171662400100615 ) ) ;
#11171 = LINE ( 'NONE', #19395, #18080 ) ;
#11172 = CARTESIAN_POINT ( 'NONE',  ( -28.68588794268871922, 417.8698905683720568, 16.75240474999999307 ) ) ;
#11173 = CARTESIAN_POINT ( 'NONE',  ( -32.66413529028185536, 234.1823905765656662, 19.99999999999999289 ) ) ;
#11174 = CARTESIAN_POINT ( 'NONE',  ( 45.67500000000000426, 4.052968581778165278E-16, -3.309499999999999886 ) ) ;
#11175 = CARTESIAN_POINT ( 'NONE',  ( -35.09675569278795848, 435.7448905683720000, 15.47720386886985366 ) ) ;
#11176 = EDGE_LOOP ( 'NONE', ( #6750, #4609, #13416, #4153, #1689, #405, #347 ) ) ;
#11177 = CARTESIAN_POINT ( 'NONE',  ( -40.53162694259545162, 472.6198905683720000, -11.84573899990672707 ) ) ;
#11178 = CARTESIAN_POINT ( 'NONE',  ( 60.03793209889851568, 36.20386280891149511, -131.1729372809869005 ) ) ;
#11179 = DIRECTION ( 'NONE',  ( 0.000000000000000000, 1.000000000000000000, 0.000000000000000000 ) ) ;
#11180 = VECTOR ( 'NONE', #11759, 1000.000000000000000 ) ;
#11181 = CARTESIAN_POINT ( 'NONE',  ( -36.33955658999051508, 373.8698905765656377, 18.47759065022572500 ) ) ;
#11182 = CARTESIAN_POINT ( 'NONE',  ( -21.75104255857543478, 45.31773601326444378, 49.11655252816966311 ) ) ;
#11183 = CARTESIAN_POINT ( 'NONE',  ( -40.01497788969913927, 370.4323905765656946, -16.95518130045146421 ) ) ;
#11184 = CARTESIAN_POINT ( 'NONE',  ( -36.33955658999051508, 430.1198905765656377, -18.47759065022572855 ) ) ;
#11185 = CARTESIAN_POINT ( 'NONE',  ( -48.68588794268886488, 252.3073905765655240, 3.978247347592742678 ) ) ;
#11186 = AXIS2_PLACEMENT_3D ( 'NONE', #14694, #14906, #14479 ) ;
#11187 = DIRECTION ( 'NONE',  ( 1.191790137725560488E-16, -1.000000000000000000, -0.000000000000000000 ) ) ;
#11188 = CARTESIAN_POINT ( 'NONE',  ( -48.68588794268852382, 256.9323905601784759, -3.978247347593583783 ) ) ;
#11189 = CARTESIAN_POINT ( 'NONE',  ( -48.68588794268870856, 347.2448905601784759, 0.000000000000000000 ) ) ;
#11190 = ADVANCED_FACE ( 'NONE', ( #11552 ), #7866, .F. ) ;
#11191 = CARTESIAN_POINT ( 'NONE',  ( -16.84014894278199392, 429.1198905683720000, 11.84573899990672530 ) ) ;
#11192 = CARTESIAN_POINT ( 'NONE',  ( -48.68588794268870856, 387.2448905601784759, 0.000000000000000000 ) ) ;
#11193 = CARTESIAN_POINT ( 'NONE',  ( -44.16309181155855867, 254.7448905683720284, -6.410867750099231266 ) ) ;
#11194 = VERTEX_POINT ( 'NONE', #6457 ) ;
#11195 = ORIENTED_EDGE ( 'NONE', *, *, #19817, .F. ) ;
#11196 = LINE ( 'NONE', #4498, #1686 ) ;
#11197 = ORIENTED_EDGE ( 'NONE', *, *, #17894, .F. ) ;
#11198 = CARTESIAN_POINT ( 'NONE',  ( -32.01814843081345430, 467.5573905683721136, 16.75240474999999307 ) ) ;
#11199 = CARTESIAN_POINT ( 'NONE',  ( -36.33955658999049376, 220.1198905765656093, -18.47759065022572855 ) ) ;
#11200 = VECTOR ( 'NONE', #16485, 999.9999999999998863 ) ;
#11201 = EDGE_CURVE ( 'NONE', #5985, #15324, #17825, .T. ) ;
#11202 = EDGE_LOOP ( 'NONE', ( #21232, #12937, #765, #6215, #9170, #2503, #13262, #17968, #3200 ) ) ;
#11203 = CARTESIAN_POINT ( 'NONE',  ( 6.416697501590670427, 172.9933428177121471, -50.00000000000000000 ) ) ;
#11204 = CARTESIAN_POINT ( 'NONE',  ( -35.09675569278793006, 221.9948905683720284, -15.47720386886985544 ) ) ;
#11205 = EDGE_CURVE ( 'NONE', #13185, #16429, #11331, .T. ) ;
#11206 = ORIENTED_EDGE ( 'NONE', *, *, #6434, .T. ) ;
#11207 = CARTESIAN_POINT ( 'NONE',  ( -40.53162694259545873, 525.1198905683720568, 11.84573899990672885 ) ) ;
#11208 = CYLINDRICAL_SURFACE ( 'NONE', #1415, 19.99999999999999645 ) ;
#11209 = EDGE_CURVE ( 'NONE', #7334, #20009, #9809, .T. ) ;
#11210 = CARTESIAN_POINT ( 'NONE',  ( -8.685887942688731655, 446.6823905765656377, 3.978247347593161010 ) ) ;
#11211 = CARTESIAN_POINT ( 'NONE',  ( 0.000000000000000000, 31.85652257517428865, 0.000000000000000000 ) ) ;
#11212 = CARTESIAN_POINT ( 'NONE',  ( 151.4788465195079823, 620.7448905601785327, -8.917803138848077182 ) ) ;
#11213 = DIRECTION ( 'NONE',  ( 0.000000000000000000, 0.000000000000000000, -1.000000000000000000 ) ) ;
#11214 = DIRECTION ( 'NONE',  ( 0.000000000000000000, 1.000000000000000000, 0.000000000000000000 ) ) ;
#11215 = CARTESIAN_POINT ( 'NONE',  ( -8.685887942688715668, 296.9948905765655809, -2.449293598294705724E-15 ) ) ;
#11216 = CARTESIAN_POINT ( 'NONE',  ( -38.17536295476243424, 235.4323905683720284, 14.20200298773971781 ) ) ;
#11217 = CARTESIAN_POINT ( 'NONE',  ( -19.19641293061497578, 308.8073905683721136, 14.20200298773971426 ) ) ;
#11218 = EDGE_CURVE ( 'NONE', #20333, #11194, #17677, .T. ) ;
#11219 = CYLINDRICAL_SURFACE ( 'NONE', #251, 4.000000000000001776 ) ;
#11220 = CARTESIAN_POINT ( 'NONE',  ( -17.35679799567829207, 380.6823905601784759, 16.95518130045146421 ) ) ;
#11221 = CARTESIAN_POINT ( 'NONE',  ( -11.93348319268871549, 300.0573905683720568, 3.332260488124728415 ) ) ;
#11222 = CARTESIAN_POINT ( 'NONE',  ( -42.88789093042843348, 362.9323905683720568, -9.489475012073736337 ) ) ;
#11223 = CARTESIAN_POINT ( 'NONE',  ( -45.43829269268873361, 525.3698905683720568, 0.000000000000000000 ) ) ;
#11224 = CARTESIAN_POINT ( 'NONE',  ( -8.685887942688720997, 361.9323905601785327, 3.978247347593161010 ) ) ;
#11225 = CARTESIAN_POINT ( 'NONE',  ( -21.03221929538692692, 404.1198905601784759, -18.47759065022572855 ) ) ;
#11226 = EDGE_LOOP ( 'NONE', ( #2438, #8750, #20599, #21208 ) ) ;
#11227 = CARTESIAN_POINT ( 'NONE',  ( -19.19641293061500065, 491.9323905683720000, -14.20200298773971603 ) ) ;
#11228 = CARTESIAN_POINT ( 'NONE',  ( -1.025382690249031503, 326.0737056351150613, -25.00000000000000000 ) ) ;
#11229 = CARTESIAN_POINT ( 'NONE',  ( -19.19641293061497933, 290.4323905683720000, -14.20200298773971603 ) ) ;
#11230 = ORIENTED_EDGE ( 'NONE', *, *, #5468, .F. ) ;
#11231 = CARTESIAN_POINT ( 'NONE',  ( -19.19641293061496867, 278.8073905683720000, 14.20200298773971426 ) ) ;
#11232 = CARTESIAN_POINT ( 'NONE',  ( -35.09675569278794427, 315.7448905683720000, 15.47720386886985366 ) ) ;
#11233 = CARTESIAN_POINT ( 'NONE',  ( -24.70764059509553334, 254.8073905765656093, 19.99999999999998934 ) ) ;
#11234 = CYLINDRICAL_SURFACE ( 'NONE', #18631, 4.000000000000001776 ) ;
#11235 = CARTESIAN_POINT ( 'NONE',  ( -45.43829269268869808, 233.8698905683720284, 0.000000000000000000 ) ) ;
#11236 = CARTESIAN_POINT ( 'NONE',  ( -16.84014894278199392, 381.6198905683720568, -11.84573899990672707 ) ) ;
#11237 = FACE_OUTER_BOUND ( 'NONE', #1362, .T. ) ;
#11238 = CARTESIAN_POINT ( 'NONE',  ( -28.68588794268875475, 600.7448905601785327, 0.000000000000000000 ) ) ;
#11239 = CARTESIAN_POINT ( 'NONE',  ( -40.01497788969913216, 270.4323905765655809, -16.95518130045146421 ) ) ;
#11240 = CARTESIAN_POINT ( 'NONE',  ( -40.53162694259544452, 415.1198905683720000, 11.84573899990672885 ) ) ;
#11241 = CARTESIAN_POINT ( 'NONE',  ( -14.31911992702480951, 600.7448905601785327, -19.70857778461545351 ) ) ;
#11242 = ORIENTED_EDGE ( 'NONE', *, *, #7755, .T. ) ;
#11243 = CARTESIAN_POINT ( 'NONE',  ( -21.03221929538691626, 420.3698905601784759, 18.47759065022572500 ) ) ;
#11244 = VERTEX_POINT ( 'NONE', #6562 ) ;
#11245 = ORIENTED_EDGE ( 'NONE', *, *, #4332, .F. ) ;
#11246 = ORIENTED_EDGE ( 'NONE', *, *, #18469, .F. ) ;
#11247 = CARTESIAN_POINT ( 'NONE',  ( -43.60132883224871847, 209.8855831874335820, -1.619299207070721502 ) ) ;
#11248 = CARTESIAN_POINT ( 'NONE',  ( -48.68588794268870146, 307.5573905601785327, 3.978247347593168115 ) ) ;
#11249 = CARTESIAN_POINT ( 'NONE',  ( -64.27068722059111394, 585.7448905601785327, 35.12437985717896538 ) ) ;
#11250 = EDGE_CURVE ( 'NONE', #21098, #2121, #19879, .T. ) ;
#11251 = CARTESIAN_POINT ( 'NONE',  ( -16.84014894278198682, 349.1198905683720568, 11.84573899990672530 ) ) ;
#11252 = CARTESIAN_POINT ( 'NONE',  ( -8.685887942688740537, 497.3073905765656377, -3.978247347593165895 ) ) ;
#11253 = CARTESIAN_POINT ( 'NONE',  ( -25.35362745456398414, 376.6823905683720000, 16.75240474999998952 ) ) ;
#11254 = PLANE ( 'NONE',  #14136 ) ;
#11255 = CARTESIAN_POINT ( 'NONE',  ( -42.88789093042844058, 392.9323905683720568, -9.489475012073734561 ) ) ;
#11256 = CARTESIAN_POINT ( 'NONE',  ( -14.54375231895776288, 325.7448905765655809, 14.14213562373094568 ) ) ;
#11257 = DIRECTION ( 'NONE',  ( 2.775557561562891844E-16, 0.000000000000000000, 1.000000000000000000 ) ) ;
#11258 = CARTESIAN_POINT ( 'NONE',  ( -14.48388495494898898, 287.9323905683720000, 9.489475012073731008 ) ) ;
#11259 =( LENGTH_UNIT ( ) NAMED_UNIT ( * ) SI_UNIT ( .MILLI., .METRE. ) );
#11260 = CARTESIAN_POINT ( 'NONE',  ( -11.93348319268872970, 440.3698905683720000, -2.051577885510841163E-15 ) ) ;
#11261 = CARTESIAN_POINT ( 'NONE',  ( -48.68588794268860909, 286.9323905601784190, -3.978247347593371508 ) ) ;
#11262 = CARTESIAN_POINT ( 'NONE',  ( -17.35679799567828852, 370.6823905601784759, 16.95518130045146421 ) ) ;
#11263 = LINE ( 'NONE', #15069, #4362 ) ;
#11264 = EDGE_CURVE ( 'NONE', #17379, #11167, #18570, .T. ) ;
#11265 = CARTESIAN_POINT ( 'NONE',  ( -16.84014894278199037, 351.6198905683720000, -11.84573899990672707 ) ) ;
#11266 = CARTESIAN_POINT ( 'NONE',  ( -32.01814843081346140, 501.6823905683720568, -16.75240474999999307 ) ) ;
#11267 = CARTESIAN_POINT ( 'NONE',  ( -28.68588794268872988, 484.7448905601784759, -19.99999999999999289 ) ) ;
#11268 = CARTESIAN_POINT ( 'NONE',  ( -25.35362745456398770, 331.0573905683720000, -16.75240474999999307 ) ) ;
#11269 = VECTOR ( 'NONE', #2955, 1000.000000000000000 ) ;
#11270 = EDGE_LOOP ( 'NONE', ( #21050, #12130, #7680, #15916 ) ) ;
#11271 = EDGE_LOOP ( 'NONE', ( #1417, #12160, #17175, #11088 ) ) ;
#11272 = FACE_OUTER_BOUND ( 'NONE', #8537, .T. ) ;
#11273 = ADVANCED_FACE ( 'NONE', ( #8724 ), #13716, .T. ) ;
#11274 = AXIS2_PLACEMENT_3D ( 'NONE', #9489, #19648, #20964 ) ;
#11275 = CARTESIAN_POINT ( 'NONE',  ( -19.19641293061498288, 398.8073905683720568, 14.20200298773971426 ) ) ;
#11276 = CYLINDRICAL_SURFACE ( 'NONE', #14904, 4.000000000000000000 ) ;
#11277 = EDGE_CURVE ( 'NONE', #15077, #4211, #19017, .T. ) ;
#11278 =( NAMED_UNIT ( * ) SI_UNIT ( $, .STERADIAN. ) SOLID_ANGLE_UNIT ( ) );
#11279 = CARTESIAN_POINT ( 'NONE',  ( -14.48388495494900674, 447.9323905683720000, 9.489475012073732785 ) ) ;
#11280 = CARTESIAN_POINT ( 'NONE',  ( -14.48388495494900852, 447.9323905683720568, 9.489475012073731008 ) ) ;
#11281 = DIRECTION ( 'NONE',  ( 0.000000000000000000, 0.000000000000000000, 1.000000000000000000 ) ) ;
#11282 = DIRECTION ( 'NONE',  ( 0.000000000000000000, 0.000000000000000000, 1.000000000000000000 ) ) ;
#11283 = CARTESIAN_POINT ( 'NONE',  ( -47.16347859291445133, 391.3698905765656377, -7.653668647301793193 ) ) ;
#11284 = CARTESIAN_POINT ( 'NONE',  ( -20.19820727147837047, 45.49892208276283156, 48.87197369005792780 ) ) ;
#11285 = CARTESIAN_POINT ( 'NONE',  ( -47.16347859291445133, 391.3698905765656377, -7.653668647301793193 ) ) ;
#11286 = CARTESIAN_POINT ( 'NONE',  ( -11.06088464903280233, 326.0737056351150613, -5.773301668816269938 ) ) ;
#11287 = DIRECTION ( 'NONE',  ( 0.9997392892938121722, 0.02283316540262222971, 0.000000000000000000 ) ) ;
#11288 = CARTESIAN_POINT ( 'NONE',  ( -35.09675569278795848, 493.4948905683720568, -15.47720386886985544 ) ) ;
#11289 = AXIS2_PLACEMENT_3D ( 'NONE', #15440, #950, #12185 ) ;
#11290 = PLANE ( 'NONE',  #16845 ) ;
#11291 = DIRECTION ( 'NONE',  ( 0.000000000000000000, 1.000000000000000000, -0.000000000000000000 ) ) ;
#11292 = CARTESIAN_POINT ( 'NONE',  ( -40.88226806564986759, 223.9102039777117170, 14.73426766465872539 ) ) ;
#11293 = ADVANCED_FACE ( 'NONE', ( #5368 ), #5479, .T. ) ;
#11294 = VECTOR ( 'NONE', #15095, 1000.000000000000114 ) ;
#11295 = CARTESIAN_POINT ( 'NONE',  ( -42.88789093042844058, 414.4323905683721136, -9.489475012073736337 ) ) ;
#11296 = CARTESIAN_POINT ( 'NONE',  ( -14.31911992702480951, 600.7448905601785327, -19.70857778461545351 ) ) ;
#11297 = CARTESIAN_POINT ( 'NONE',  ( -42.88789093042841927, 246.3073905683720284, 9.489475012073736337 ) ) ;
#11298 = VERTEX_POINT ( 'NONE', #633 ) ;
#11299 = DIRECTION ( 'NONE',  ( -0.000000000000000000, -1.000000000000000000, -0.000000000000000000 ) ) ;
#11300 = VERTEX_POINT ( 'NONE', #10235 ) ;
#11301 = CARTESIAN_POINT ( 'NONE',  ( -16.84014894278199748, 459.1198905683720568, 11.84573899990672530 ) ) ;
#11302 = CARTESIAN_POINT ( 'NONE',  ( -45.43829269268872650, 533.5573905683720568, -3.332260488124726194 ) ) ;
#11303 = AXIS2_PLACEMENT_3D ( 'NONE', #21352, #11389, #3186 ) ;
#11304 = VERTEX_POINT ( 'NONE', #12079 ) ;
#11305 = CARTESIAN_POINT ( 'NONE',  ( -43.68588794268869435, 210.1437886375728965, 2.161863591991830530E-19 ) ) ;
#11306 = CARTESIAN_POINT ( 'NONE',  ( -11.93348319268870483, 228.8698905683720284, -2.051577885510841163E-15 ) ) ;
#11307 = ORIENTED_EDGE ( 'NONE', *, *, #8765, .T. ) ;
#11308 = CARTESIAN_POINT ( 'NONE',  ( -28.68588794268872988, 506.3698905683720000, 16.75240474999999307 ) ) ;
#11309 = CARTESIAN_POINT ( 'NONE',  ( 68.91750629823305019, 180.5807618359183664, -53.41772401313671992 ) ) ;
#11310 = CIRCLE ( 'NONE', #8196, 15.00000000000000000 ) ;
#11311 = CARTESIAN_POINT ( 'NONE',  ( -10.20829729246299600, 447.6198905765656377, -7.653668647301794969 ) ) ;
#11312 = PRODUCT_DEFINITION_SHAPE ( 'NONE', 'NONE',  #21393 ) ;
#11313 = CARTESIAN_POINT ( 'NONE',  ( -45.64106924314017277, 301.0573905765655809, -11.32908994701042538 ) ) ;
#11314 = CARTESIAN_POINT ( 'NONE',  ( -14.48388495494899608, 337.9323905683720568, 9.489475012073731008 ) ) ;
#11315 = CARTESIAN_POINT ( 'NONE',  ( -203.6858879426887654, 610.7448905601785327, 2.143131898507868248E-14 ) ) ;
#11316 = CARTESIAN_POINT ( 'NONE',  ( -28.68588794268874054, 573.2448905601785327, 0.000000000000000000 ) ) ;
#11317 = B_SPLINE_CURVE_WITH_KNOTS ( 'NONE', 3,
 ( #19815, #9847, #18183, #19918, #16260, #8008 ),
 .UNSPECIFIED., .F., .F.,
 ( 4, 2, 4 ),
 ( 0.01913986446880883499, 0.02104055318064342039, 0.02294124189247800580 ),
 .UNSPECIFIED. ) ;
#11318 = CARTESIAN_POINT ( 'NONE',  ( -35.86044580198795018, 223.9104597372275123, 18.66884633871304899 ) ) ;
#11319 = CARTESIAN_POINT ( 'NONE',  ( -11.93348319268870483, 228.8698905683720284, -2.051577885510841163E-15 ) ) ;
#11320 = CARTESIAN_POINT ( 'NONE',  ( -35.09675569278794427, 317.2448905683720000, 15.47720386886985366 ) ) ;
#11321 = PLANE ( 'NONE',  #12664 ) ;
#11322 = CARTESIAN_POINT ( 'NONE',  ( -48.68588794268870146, 276.9323905601784190, -3.978247347593158345 ) ) ;
#11323 = CARTESIAN_POINT ( 'NONE',  ( -32.66413529028186957, 379.4323905601785327, 19.99999999999999289 ) ) ;
#11324 = ADVANCED_FACE ( 'NONE', ( #10026 ), #6781, .T. ) ;
#11325 = CARTESIAN_POINT ( 'NONE',  ( -22.27502019258946930, 308.4948905683720568, 15.47720386886985189 ) ) ;
#11326 = CARTESIAN_POINT ( 'NONE',  ( -44.16309181155859420, 514.7448905683720568, -6.410867750099231266 ) ) ;
#11327 = CARTESIAN_POINT ( 'NONE',  ( -32.66413529028187668, 365.0573905601784759, -19.99999999999999289 ) ) ;
#11328 = DIRECTION ( 'NONE',  ( -1.000000000000000000, -0.000000000000000000, -0.000000000000000000 ) ) ;
#11329 = ORIENTED_EDGE ( 'NONE', *, *, #21176, .F. ) ;
#11330 = CARTESIAN_POINT ( 'NONE',  ( -11.93348319268873681, 490.3698905683720568, -2.051577885510841163E-15 ) ) ;
#11331 = LINE ( 'NONE', #17926, #15624 ) ;
#11332 = CARTESIAN_POINT ( 'NONE',  ( -32.01814843081344009, 281.6823905683720568, -16.75240474999999307 ) ) ;
#11333 = ORIENTED_EDGE ( 'NONE', *, *, #1654, .F. ) ;
#11334 = EDGE_CURVE ( 'NONE', #13635, #4322, #13186, .T. ) ;
#11335 = CARTESIAN_POINT ( 'NONE',  ( -38.17536295476244135, 286.9323905683720000, 14.20200298773971781 ) ) ;
#11336 = CARTESIAN_POINT ( 'NONE',  ( -25.35362745456398770, 331.0573905683720000, -16.75240474999999307 ) ) ;
#11337 = CARTESIAN_POINT ( 'NONE',  ( -11.93348319268870839, 260.3698905683720000, -2.051577885510841163E-15 ) ) ;
#11338 =( BOUNDED_CURVE ( )  B_SPLINE_CURVE ( 2, ( #14340, #20920, #16382, #371, #160, #10080, #11495, #11920, #3394, #18092, #15082, #11712, #16592, #1890, #6619, #13240, #18411 ),
 .UNSPECIFIED., .F., .T. ) 
 B_SPLINE_CURVE_WITH_KNOTS ( ( 3, 2, 2, 2, 2, 2, 2, 2, 3 ),
 ( 0.2656250000000002220, 0.2675781250000002220, 0.2695312500000001665, 0.2714843750000001665, 0.2734375000000001110, 0.2753906250000001110, 0.2773437500000001110, 0.2792968750000000555, 0.2812500000000000555 ),
 .UNSPECIFIED. ) 
 CURVE ( )  GEOMETRIC_REPRESENTATION_ITEM ( )  RATIONAL_B_SPLINE_CURVE ( ( 0.9999999999999977796, 0.9807852804032326510, 1.000000000000000000, 0.9807852804032304306, 1.000000000000000000, 0.9807852804032304306, 1.000000000000000000, 0.9807852804032304306, 1.000000000000000000, 0.9807852804032304306, 1.000000000000000000, 0.9807852804032304306, 1.000000000000000000, 0.9807852804032304306, 1.000000000000000000, 0.9807852804032298755, 1.000000000000000444 ) ) 
 REPRESENTATION_ITEM ( '' )  );
#11339 = CARTESIAN_POINT ( 'NONE',  ( -36.33955658999050087, 270.1198905765655809, -18.47759065022572855 ) ) ;
#11340 = CARTESIAN_POINT ( 'NONE',  ( -8.685887942688548691, 392.5573905601785327, -3.978247347592740013 ) ) ;
#11341 = CARTESIAN_POINT ( 'NONE',  ( -45.35320578180308360, 224.2032419181830107, 3.537678462365220877 ) ) ;
#11342 = CARTESIAN_POINT ( 'NONE',  ( -28.68588794268871212, 367.8698905683720000, 16.75240474999999307 ) ) ;
#11343 = CARTESIAN_POINT ( 'NONE',  ( -8.685887942688712116, 282.2448905601784759, -2.449293598294705724E-15 ) ) ;
#11344 = CARTESIAN_POINT ( 'NONE',  ( 2.416697501590669095, 217.7548513357008630, -49.99999999999999289 ) ) ;
#11345 = CARTESIAN_POINT ( 'NONE',  ( 4.700000000000000178, 5.629165124598848102, -3.250000000000007994 ) ) ;
#11346 = CARTESIAN_POINT ( 'NONE',  ( -25.35362745456399836, 431.0573905683720000, -16.75240474999999307 ) ) ;
#11347 = LINE ( 'NONE', #4970, #20000 ) ;
#11348 = VERTEX_POINT ( 'NONE', #18250 ) ;
#11349 = CARTESIAN_POINT ( 'NONE',  ( -40.01497788969914637, 435.6823905601784759, -16.95518130045146421 ) ) ;
#11350 = EDGE_LOOP ( 'NONE', ( #20521, #6191, #17615, #13538 ) ) ;
#11351 = ORIENTED_EDGE ( 'NONE', *, *, #18350, .F. ) ;
#11352 = ORIENTED_EDGE ( 'NONE', *, *, #11004, .T. ) ;
#11353 = FACE_OUTER_BOUND ( 'NONE', #15209, .T. ) ;
#11354 = CARTESIAN_POINT ( 'NONE',  ( -21.03221929538690205, 300.3698905601784759, 18.47759065022572500 ) ) ;
#11355 = CYLINDRICAL_SURFACE ( 'NONE', #9716, 20.00000000000000355 ) ;
#11356 = CARTESIAN_POINT ( 'NONE',  ( -22.27502019258947286, 338.4948905683720568, 15.47720386886985189 ) ) ;
#11357 = CARTESIAN_POINT ( 'NONE',  ( -32.66413529028189089, 494.1823905765655240, 19.99999999999999289 ) ) ;
#11358 = CARTESIAN_POINT ( 'NONE',  ( -22.27502019258947996, 386.9948905683720568, 15.47720386886985189 ) ) ;
#11359 = DIRECTION ( 'NONE',  ( 0.000000000000000000, 0.000000000000000000, -1.000000000000000000 ) ) ;
#11360 = CARTESIAN_POINT ( 'NONE',  ( -25.35362745456398414, 376.6823905683720000, 16.75240474999998952 ) ) ;
#11361 = AXIS2_PLACEMENT_3D ( 'NONE', #17259, #832, #14451 ) ;
#11362 = CARTESIAN_POINT ( 'NONE',  ( -17.35679799567829562, 328.5573905765656377, -16.95518130045146421 ) ) ;
#11363 = CARTESIAN_POINT ( 'NONE',  ( -54.57497958038185004, 303.6587712403113528, 49.99999999999999289 ) ) ;
#11364 = CARTESIAN_POINT ( 'NONE',  ( -35.09675569278793716, 291.9948905683720000, -15.47720386886985544 ) ) ;
#11365 = CARTESIAN_POINT ( 'NONE',  ( -16.84014894278199748, 439.1198905683720568, 11.84573899990672530 ) ) ;
#11366 = CARTESIAN_POINT ( 'NONE',  ( 0.000000000000000000, 610.7448905601785327, 0.000000000000000000 ) ) ;
#11367 = DIRECTION ( 'NONE',  ( 0.000000000000000000, 1.000000000000000000, 0.000000000000000000 ) ) ;
#11368 = VECTOR ( 'NONE', #7819, 1000.000000000000000 ) ;
#11369 = FACE_OUTER_BOUND ( 'NONE', #19529, .T. ) ;
#11370 = CARTESIAN_POINT ( 'NONE',  ( 8.938426032941704028E-16, 585.7448905601785327, -7.500000000000000000 ) ) ;
#11371 = CARTESIAN_POINT ( 'NONE',  ( -14.48388495494899608, 349.4323905683720000, 9.489475012073732785 ) ) ;
#11372 = CARTESIAN_POINT ( 'NONE',  ( -28.68588794268872988, 481.3698905683720568, -16.75240474999999307 ) ) ;
#11373 = CARTESIAN_POINT ( 'NONE',  ( -48.68588794268872277, 477.5573905601784759, 3.978247347593168115 ) ) ;
#11374 = CARTESIAN_POINT ( 'NONE',  ( -28.68588794268870856, 326.3698905683720000, 16.75240474999999307 ) ) ;
#11375 = AXIS2_PLACEMENT_3D ( 'NONE', #20132, #2071, #245 ) ;
#11376 = ORIENTED_EDGE ( 'NONE', *, *, #20200, .F. ) ;
#11377 = CARTESIAN_POINT ( 'NONE',  ( -38.86787825240671168, 223.9102039777116318, -13.30301237467029019 ) ) ;
#11378 = VERTEX_POINT ( 'NONE', #20415 ) ;
#11379 = CARTESIAN_POINT ( 'NONE',  ( 5.299999999999999822, -7.505553499465150047, 0.000000000000000000 ) ) ;
#11380 = EDGE_CURVE ( 'NONE', #10794, #10285, #11659, .T. ) ;
#11381 = CARTESIAN_POINT ( 'NONE',  ( -35.09675569278795848, 407.2448905683720568, 15.47720386886985366 ) ) ;
#11382 = CARTESIAN_POINT ( 'NONE',  ( -48.68588794268870856, 357.2448905601784759, 0.000000000000000000 ) ) ;
#11383 = LINE ( 'NONE', #12702, #8645 ) ;
#11384 = CARTESIAN_POINT ( 'NONE',  ( -28.68588794268872633, 441.3698905683720000, -16.75240474999999307 ) ) ;
#11385 = CARTESIAN_POINT ( 'NONE',  ( -45.43829269268871940, 443.5573905683719431, -3.332260488124726638 ) ) ;
#11386 = CARTESIAN_POINT ( 'NONE',  ( -11.73070664223725501, 413.1823905601784190, -11.32908994701042538 ) ) ;
#11387 = CARTESIAN_POINT ( 'NONE',  ( -14.54375231895776999, 385.7448905765656377, 14.14213562373094568 ) ) ;
#11388 = DIRECTION ( 'NONE',  ( -0.000000000000000000, -1.000000000000000000, -0.000000000000000000 ) ) ;
#11389 = DIRECTION ( 'NONE',  ( -1.191790137725560488E-16, 1.000000000000000000, -0.000000000000000000 ) ) ;
#11390 = DIRECTION ( 'NONE',  ( -1.000000000000000000, 0.000000000000000000, -0.000000000000000000 ) ) ;
#11391 = CARTESIAN_POINT ( 'NONE',  ( -20.54277306141298354, 600.7448905601785327, -49.33244044267773631 ) ) ;
#11392 = CARTESIAN_POINT ( 'NONE',  ( -32.01814843081346140, 503.1823905683721136, -16.75240474999999307 ) ) ;
#11393 = DIRECTION ( 'NONE',  ( 1.191790137725560488E-16, -1.000000000000000000, -0.000000000000000000 ) ) ;
#11394 = DIRECTION ( 'NONE',  ( -1.191790137725560488E-16, 1.000000000000000000, -0.000000000000000000 ) ) ;
#11395 = CARTESIAN_POINT ( 'NONE',  ( -8.685887942688740537, 522.2448905601784190, -2.449293598294705724E-15 ) ) ;
#11396 =( BOUNDED_CURVE ( )  B_SPLINE_CURVE ( 2, ( #2848, #9001, #14431, #7697, #14107, #20692, #19383, #2740, #5865, #19279, #5972, #6181, #4568, #19177, #7798, #12474, #14326 ),
 .UNSPECIFIED., .F., .T. ) 
 B_SPLINE_CURVE_WITH_KNOTS ( ( 3, 2, 2, 2, 2, 2, 2, 2, 3 ),
 ( 0.2343750000000001943, 0.2363281250000001943, 0.2382812500000001943, 0.2402343750000001943, 0.2421875000000002220, 0.2441406250000002220, 0.2460937500000002220, 0.2480468750000002220, 0.2500000000000002220 ),
 .UNSPECIFIED. ) 
 CURVE ( )  GEOMETRIC_REPRESENTATION_ITEM ( )  RATIONAL_B_SPLINE_CURVE ( ( 0.9999999999999981126, 0.9807852804032323180, 1.000000000000000000, 0.9807852804032304306, 1.000000000000000000, 0.9807852804032304306, 1.000000000000000000, 0.9807852804032304306, 1.000000000000000000, 0.9807852804032304306, 1.000000000000000000, 0.9807852804032304306, 1.000000000000000000, 0.9807852804032304306, 1.000000000000000000, 0.9807852804032282101, 1.000000000000002220 ) ) 
 REPRESENTATION_ITEM ( '' )  );
#11397 = ADVANCED_FACE ( 'NONE', ( #13616 ), #20100, .T. ) ;
#11398 = CARTESIAN_POINT ( 'NONE',  ( -32.01814843081345430, 403.1823905683720000, -16.75240474999999307 ) ) ;
#11399 = CARTESIAN_POINT ( 'NONE',  ( -24.70764059509557242, 469.1823905765656377, -19.99999999999999289 ) ) ;
#11400 = CARTESIAN_POINT ( 'NONE',  ( -48.68588794268872988, 537.2448905601785327, 0.000000000000000000 ) ) ;
#11401 = VERTEX_POINT ( 'NONE', #11874 ) ;
#11402 = CARTESIAN_POINT ( 'NONE',  ( -123.2946569474810161, 10.52886280891152104, 20.57735571454641388 ) ) ;
#11403 = ORIENTED_EDGE ( 'NONE', *, *, #210, .F. ) ;
#11404 = CARTESIAN_POINT ( 'NONE',  ( -16.84014894278200103, 469.1198905683720568, 11.84573899990672530 ) ) ;
#11405 = CARTESIAN_POINT ( 'NONE',  ( -8.685887942688708563, 236.6823905765656093, 3.978247347593161010 ) ) ;
#11406 = EDGE_LOOP ( 'NONE', ( #9830, #4655, #1938, #321, #9283, #11459 ) ) ;
#11407 = DIRECTION ( 'NONE',  ( -0.000000000000000000, -0.000000000000000000, -1.000000000000000000 ) ) ;
#11408 = CARTESIAN_POINT ( 'NONE',  ( -35.09675569278797269, 527.2448905683719431, 15.47720386886985366 ) ) ;
#11409 = VERTEX_POINT ( 'NONE', #18464 ) ;
#11410 = CARTESIAN_POINT ( 'NONE',  ( -28.68588794268873343, 511.3698905683720000, -16.75240474999999307 ) ) ;
#11411 = DIRECTION ( 'NONE',  ( 0.000000000000000000, -1.000000000000000000, 0.000000000000000000 ) ) ;
#11412 = EDGE_CURVE ( 'NONE', #9723, #12542, #3752, .T. ) ;
#11413 = CIRCLE ( 'NONE', #741, 6.500000000000000888 ) ;
#11415 = AXIS2_PLACEMENT_3D ( 'NONE', #20345, #5519, #12660 ) ;
#11414 = CARTESIAN_POINT ( 'NONE',  ( -24.70764059509557242, 449.1823905765655809, -19.99999999999999289 ) ) ;
#11416 = DIRECTION ( 'NONE',  ( 0.000000000000000000, 0.000000000000000000, 1.000000000000000000 ) ) ;
#11417 = LINE ( 'NONE', #19971, #280 ) ;
#11418 = CARTESIAN_POINT ( 'NONE',  ( -11.73070664223725856, 456.0573905765655809, 11.32908994701042005 ) ) ;
#11419 = CIRCLE ( 'NONE', #19713, 5.000000000000001776 ) ;
#11420 = FACE_OUTER_BOUND ( 'NONE', #20407, .T. ) ;
#11421 = DIRECTION ( 'NONE',  ( 0.000000000000000000, 0.000000000000000000, -1.000000000000000000 ) ) ;
#11422 = CARTESIAN_POINT ( 'NONE',  ( -31.26501780185373391, 205.1437886375728965, 0.000000000000000000 ) ) ;
#11423 = PLANE ( 'NONE',  #14914 ) ;
#11424 = CARTESIAN_POINT ( 'NONE',  ( -11.93348319268871727, 310.6823905683720568, -3.332260488124732856 ) ) ;
#11425 = EDGE_CURVE ( 'NONE', #15685, #12221, #2042, .T. ) ;
#11426 = LINE ( 'NONE', #6553, #2643 ) ;
#11427 = CARTESIAN_POINT ( 'NONE',  ( -48.68588794268869435, 266.9323905601784759, -3.978247347593158345 ) ) ;
#11428 = CARTESIAN_POINT ( 'NONE',  ( 65.85920792673738333, 160.1716627696692683, -40.00000000000000000 ) ) ;
#11429 = CARTESIAN_POINT ( 'NONE',  ( -32.01814843081344009, 283.1823905683720568, -16.75240474999999307 ) ) ;
#11430 = AXIS2_PLACEMENT_3D ( 'NONE', #19399, #14341, #21345 ) ;
#11431 = VECTOR ( 'NONE', #18211, 1000.000000000000000 ) ;
#11432 = CARTESIAN_POINT ( 'NONE',  ( -44.16309181155858710, 515.9948905683720568, 6.410867750099241924 ) ) ;
#11433 = CARTESIAN_POINT ( 'NONE',  ( -40.01497788969913216, 358.8073905601784190, 16.95518130045146776 ) ) ;
#11434 = CARTESIAN_POINT ( 'NONE',  ( -28.68588794268872277, 378.8848358243226357, 20.00000000000000000 ) ) ;
#11435 = ORIENTED_EDGE ( 'NONE', *, *, #2847, .T. ) ;
#11436 = CARTESIAN_POINT ( 'NONE',  ( -45.43829269268871940, 495.0573905683719431, -3.332260488124726194 ) ) ;
#11437 = CYLINDRICAL_SURFACE ( 'NONE', #5925, 11.54039041455135184 ) ;
#11438 = CARTESIAN_POINT ( 'NONE',  ( -13.20868407381885135, 289.4948905683720000, -6.410867750099233042 ) ) ;
#11439 = ORIENTED_EDGE ( 'NONE', *, *, #6774, .F. ) ;
#11440 = CARTESIAN_POINT ( 'NONE',  ( -45.43829269268870519, 275.6823905683720000, 3.332260488124734632 ) ) ;
#11441 = CARTESIAN_POINT ( 'NONE',  ( -42.88789093042842637, 312.9323905683720000, -9.489475012073736337 ) ) ;
#11442 = CARTESIAN_POINT ( 'NONE',  ( -40.53162694259542320, 256.6198905683720568, 11.84573899990672885 ) ) ;
#11443 = CARTESIAN_POINT ( 'NONE',  ( -14.54375231895775578, 238.2448905765656093, -14.14213562373094746 ) ) ;
#11444 = DIRECTION ( 'NONE',  ( -1.000000000000000000, 0.000000000000000000, 0.000000000000000000 ) ) ;
#11445 = AXIS2_PLACEMENT_3D ( 'NONE', #9918, #4634, #8078 ) ;
#11446 = DIRECTION ( 'NONE',  ( 0.3512089204514979301, 0.000000000000000000, -0.9362971185447991340 ) ) ;
#11447 = CARTESIAN_POINT ( 'NONE',  ( -14.48388495494900141, 371.3073905683720568, -9.489475012073736337 ) ) ;
#11448 = DIRECTION ( 'NONE',  ( -1.000000000000000000, 0.000000000000000000, 0.000000000000000000 ) ) ;
#11449 = DIRECTION ( 'NONE',  ( 0.000000000000000000, 0.000000000000000000, -1.000000000000000000 ) ) ;
#11450 = EDGE_CURVE ( 'NONE', #9674, #1161, #15238, .T. ) ;
#11451 = CARTESIAN_POINT ( 'NONE',  ( -42.82802356641965247, 270.7448905765656377, -14.14213562373094746 ) ) ;
#11452 = ADVANCED_FACE ( 'NONE', ( #17384 ), #12192, .T. ) ;
#11453 = CARTESIAN_POINT ( 'NONE',  ( -11.93348319268872793, 418.5573905683720568, 3.332260488124728415 ) ) ;
#11454 = FACE_OUTER_BOUND ( 'NONE', #20010, .T. ) ;
#11455 = ORIENTED_EDGE ( 'NONE', *, *, #9347, .F. ) ;
#11456 = CARTESIAN_POINT ( 'NONE',  ( -28.68588794268872277, 434.7448905601784759, -19.99999999999999289 ) ) ;
#11457 = ORIENTED_EDGE ( 'NONE', *, *, #8372, .F. ) ;
#11458 = DIRECTION ( 'NONE',  ( 0.000000000000000000, 0.000000000000000000, 1.000000000000000000 ) ) ;
#11459 = ORIENTED_EDGE ( 'NONE', *, *, #6703, .F. ) ;
#11460 = ORIENTED_EDGE ( 'NONE', *, *, #7088, .F. ) ;
#11461 = CARTESIAN_POINT ( 'NONE',  ( -40.01497788969913216, 353.5573905765656377, 16.95518130045146776 ) ) ;
#11462 = CARTESIAN_POINT ( 'NONE',  ( -47.16347859291443712, 296.6198905601784759, -7.653668647301793193 ) ) ;
#11463 = FACE_OUTER_BOUND ( 'NONE', #16159, .T. ) ;
#11464 =( GEOMETRIC_REPRESENTATION_CONTEXT ( 3 ) GLOBAL_UNCERTAINTY_ASSIGNED_CONTEXT ( ( #8092 ) ) GLOBAL_UNIT_ASSIGNED_CONTEXT ( ( #20718, #2341, #621 ) ) REPRESENTATION_CONTEXT ( 'NONE', 'WORKASPACE' ) );
#11465 = ADVANCED_FACE ( 'NONE', ( #14259 ), #19112, .T. ) ;
#11466 = CARTESIAN_POINT ( 'NONE',  ( -45.43829269268871229, 335.6823905683720568, 3.332260488124734632 ) ) ;
#11467 = CARTESIAN_POINT ( 'NONE',  ( -11.73070664223726034, 476.0573905765656377, 11.32908994701042005 ) ) ;
#11468 = CARTESIAN_POINT ( 'NONE',  ( -44.16309181155857289, 363.2448905683720000, -6.410867750099231266 ) ) ;
#11469 = CARTESIAN_POINT ( 'NONE',  ( -45.64106924314017277, 311.0573905765656377, -11.32908994701042538 ) ) ;
#11470 = CARTESIAN_POINT ( 'NONE',  ( -14.48388495494900141, 379.8073905683721136, -9.489475012073734561 ) ) ;
#11471 = EDGE_CURVE ( 'NONE', #10685, #15951, #15559, .T. ) ;
#11472 = CARTESIAN_POINT ( 'NONE',  ( -28.68588794268870856, 324.4948905765655809, 19.99999999999999289 ) ) ;
#11473 = LINE ( 'NONE', #11154, #12422 ) ;
#11474 = CARTESIAN_POINT ( 'NONE',  ( -11.93348319268871194, 279.1823905683720000, -3.332260488124732856 ) ) ;
#11475 = PLANE ( 'NONE',  #14312 ) ;
#11476 = AXIS2_PLACEMENT_3D ( 'NONE', #3637, #6765, #3736 ) ;
#11477 = CARTESIAN_POINT ( 'NONE',  ( -11.93348319268872970, 430.6823905683720568, -3.332260488124732856 ) ) ;
#11478 = CARTESIAN_POINT ( 'NONE',  ( -17.35679799567828496, 283.8073905601784759, -16.95518130045146421 ) ) ;
#11479 = CARTESIAN_POINT ( 'NONE',  ( -28.68588794268873343, 514.7448905601784190, -19.99999999999999289 ) ) ;
#11480 = DIRECTION ( 'NONE',  ( -1.000000000000000000, -0.000000000000000000, -0.000000000000000000 ) ) ;
#11481 = AXIS2_PLACEMENT_3D ( 'NONE', #20674, #14310, #20893 ) ;
#11482 = CARTESIAN_POINT ( 'NONE',  ( -42.82802356641966668, 448.4948905601784759, 14.14213562373094923 ) ) ;
#11483 = EDGE_CURVE ( 'NONE', #10958, #289, #18780, .T. ) ;
#11484 = CARTESIAN_POINT ( 'NONE',  ( -16.84014894278198327, 339.1198905683720568, 11.84573899990672530 ) ) ;
#11485 = CARTESIAN_POINT ( 'NONE',  ( -45.43829269268871940, 483.5573905683720000, -3.332260488124726194 ) ) ;
#11486 = ORIENTED_EDGE ( 'NONE', *, *, #13604, .T. ) ;
#11487 = CARTESIAN_POINT ( 'NONE',  ( -14.54375231895778064, 480.9948905601784759, 14.14213562373094568 ) ) ;
#11488 = CARTESIAN_POINT ( 'NONE',  ( -40.53162694259543031, 295.1198905683720000, 11.84573899990672885 ) ) ;
#11489 = EDGE_LOOP ( 'NONE', ( #2831, #10045, #18929, #7198 ) ) ;
#11490 = LINE ( 'NONE', #21125, #1084 ) ;
#11491 = ORIENTED_EDGE ( 'NONE', *, *, #9876, .F. ) ;
#11492 = CARTESIAN_POINT ( 'NONE',  ( -28.68588794268874054, 573.2448905601785327, 0.000000000000000000 ) ) ;
#11493 = VECTOR ( 'NONE', #10382, 1000.000000000000000 ) ;
#11494 = CARTESIAN_POINT ( 'NONE',  ( -38.17536295476246266, 413.8073905683719431, -14.20200298773971426 ) ) ;
#11495 = CARTESIAN_POINT ( 'NONE',  ( -21.03221929538691981, 445.1198905765655809, 18.47759065022572500 ) ) ;
#11496 = CARTESIAN_POINT ( 'NONE',  ( 81.24038404635966515, 56.85652257517428865, -94.99999999999994316 ) ) ;
#11497 = CARTESIAN_POINT ( 'NONE',  ( -14.48388495494900496, 437.9323905683720000, 9.489475012073732785 ) ) ;
#11498 = CARTESIAN_POINT ( 'NONE',  ( -11.93348319268872970, 439.1823905683720000, -3.332260488124732856 ) ) ;
#11499 = SHAPE_DEFINITION_REPRESENTATION ( #965, #15840 ) ;
#11500 = CARTESIAN_POINT ( 'NONE',  ( -40.01497788969913927, 398.8073905601784759, 16.95518130045146776 ) ) ;
#11501 = CARTESIAN_POINT ( 'NONE',  ( -45.64106924314018698, 382.9323905765656377, 11.32908994701042715 ) ) ;
#11502 = CARTESIAN_POINT ( 'NONE',  ( -26.36169529657598076, 46.03899998623287360, 49.54893611991261793 ) ) ;
#11503 = CARTESIAN_POINT ( 'NONE',  ( -47.16347859291443001, 266.6198905601784759, -7.653668647301793193 ) ) ;
#11504 = DIRECTION ( 'NONE',  ( 0.000000000000000000, -1.000000000000000000, 0.000000000000000000 ) ) ;
#11505 = DIRECTION ( 'NONE',  ( 1.191790137725560488E-16, -1.000000000000000000, -0.000000000000000000 ) ) ;
#11506 = CARTESIAN_POINT ( 'NONE',  ( -40.53162694259545162, 494.1198905683720000, -11.84573899990672707 ) ) ;
#11507 = VECTOR ( 'NONE', #18509, 1000.000000000000000 ) ;
#11508 = LINE ( 'NONE', #6414, #5072 ) ;
#11509 = CARTESIAN_POINT ( 'NONE',  ( -14.54375231895778242, 463.4948905601785327, -14.14213562373094746 ) ) ;
#11510 = EDGE_CURVE ( 'NONE', #4211, #12773, #6016, .T. ) ;
#11511 = CARTESIAN_POINT ( 'NONE',  ( -48.68588794268871567, 417.2448905601784759, 0.000000000000000000 ) ) ;
#11512 = VECTOR ( 'NONE', #19466, 1000.000000000000000 ) ;
#11513 = CARTESIAN_POINT ( 'NONE',  ( -32.01814843081345430, 407.5573905683720568, 16.75240474999999307 ) ) ;
#11514 = CARTESIAN_POINT ( 'NONE',  ( -40.01497788969911795, 263.5573905765656377, 16.95518130045146776 ) ) ;
#11515 = ADVANCED_BREP_SHAPE_REPRESENTATION ( '', ( #12085, #12794 ), #4502 ) ;
#11516 = CARTESIAN_POINT ( 'NONE',  ( -45.43829269268869808, 225.3698905683720284, 0.000000000000000000 ) ) ;
#11517 = ORIENTED_EDGE ( 'NONE', *, *, #9958, .F. ) ;
#11518 = FACE_OUTER_BOUND ( 'NONE', #11086, .T. ) ;
#11519 = ORIENTED_EDGE ( 'NONE', *, *, #13996, .F. ) ;
#11520 = CARTESIAN_POINT ( 'NONE',  ( -40.53162694259544452, 444.1198905683720568, -11.84573899990672707 ) ) ;
#11521 = CARTESIAN_POINT ( 'NONE',  ( -19.19641293061500420, 530.4323905683720568, -14.20200298773971603 ) ) ;
#11522 = VECTOR ( 'NONE', #423, 1000.000000000000000 ) ;
#11523 = ORIENTED_EDGE ( 'NONE', *, *, #8682, .T. ) ;
#11524 = CARTESIAN_POINT ( 'NONE',  ( -42.82802356641964536, 205.1437886375728965, 5.000000000000001776 ) ) ;
#11525 = CARTESIAN_POINT ( 'NONE',  ( -22.27502019258946930, 220.7448905683720568, -15.47720386886985544 ) ) ;
#11526 = ORIENTED_EDGE ( 'NONE', *, *, #20326, .F. ) ;
#11527 = CARTESIAN_POINT ( 'NONE',  ( -25.35362745456400901, 501.0573905683720568, -16.75240474999999307 ) ) ;
#11528 = CARTESIAN_POINT ( 'NONE',  ( -162.2727221670389781, 30.52886280891152282, 4.999999999999990230 ) ) ;
#11529 = AXIS2_PLACEMENT_3D ( 'NONE', #2577, #5698, #15566 ) ;
#11530 = ADVANCED_FACE ( 'NONE', ( #9147 ), #4399, .T. ) ;
#11531 = CARTESIAN_POINT ( 'NONE',  ( -14.54375231895778064, 438.2448905765656377, -14.14213562373094746 ) ) ;
#11532 = CARTESIAN_POINT ( 'NONE',  ( 0.4042117618287672243, -3.141900367811076400, 6.500000000000000000 ) ) ;
#11533 = CARTESIAN_POINT ( 'NONE',  ( -42.82802356641964536, 250.7448905765656377, -14.14213562373094746 ) ) ;
#11534 = CARTESIAN_POINT ( 'NONE',  ( -28.68588794268872277, 454.4948905765656377, 19.99999999999999289 ) ) ;
#11535 = CARTESIAN_POINT ( 'NONE',  ( 0.2573354458087862007, -4.368923434677201456, -5.432802636760778903 ) ) ;
#11536 = CARTESIAN_POINT ( 'NONE',  ( -11.73070664223723725, 291.3073905601785327, 11.32908994701042005 ) ) ;
#11537 =( BOUNDED_CURVE ( )  B_SPLINE_CURVE ( 2, ( #5461, #8494, #8814, #5354, #12175, #18762, #302, #15539, #5255, #3950, #10535, #7292, #8708, #20506, #5676, #12283, #18864 ),
 .UNSPECIFIED., .F., .T. ) 
 B_SPLINE_CURVE_WITH_KNOTS ( ( 3, 2, 2, 2, 2, 2, 2, 2, 3 ),
 ( 0.1562500000000001388, 0.1582031250000001388, 0.1601562500000001388, 0.1621093750000001388, 0.1640625000000001665, 0.1660156250000001665, 0.1679687500000001665, 0.1699218750000001665, 0.1718750000000001665 ),
 .UNSPECIFIED. ) 
 CURVE ( )  GEOMETRIC_REPRESENTATION_ITEM ( )  RATIONAL_B_SPLINE_CURVE ( ( 0.9999999999999986677, 0.9807852804032317628, 1.000000000000000000, 0.9807852804032304306, 1.000000000000000000, 0.9807852804032304306, 1.000000000000000000, 0.9807852804032304306, 1.000000000000000000, 0.9807852804032304306, 1.000000000000000000, 0.9807852804032304306, 1.000000000000000000, 0.9807852804032304306, 1.000000000000000000, 0.9807852804032287652, 1.000000000000001554 ) ) 
 REPRESENTATION_ITEM ( '' )  );
#11538 = CYLINDRICAL_SURFACE ( 'NONE', #11808, 4.000000000000001776 ) ;
#11539 = CARTESIAN_POINT ( 'NONE',  ( 91.21585410611801592, 31.85652257517428865, 85.46735025547120301 ) ) ;
#11540 = CARTESIAN_POINT ( 'NONE',  ( -38.17536295476244845, 323.8073905683719431, -14.20200298773971426 ) ) ;
#11541 = FACE_OUTER_BOUND ( 'NONE', #11687, .T. ) ;
#11542 = CARTESIAN_POINT ( 'NONE',  ( -11.73070664223723547, 271.3073905601785327, 11.32908994701042005 ) ) ;
#11543 = CARTESIAN_POINT ( 'NONE',  ( -10.76731745429009912, 50.09631838541057647, -118.3724535612433186 ) ) ;
#11544 = VECTOR ( 'NONE', #13561, 1000.000000000000000 ) ;
#11545 = CARTESIAN_POINT ( 'NONE',  ( -32.01814843081344009, 297.5573905683720000, 16.75240474999999307 ) ) ;
#11546 = EDGE_CURVE ( 'NONE', #16325, #17928, #7523, .T. ) ;
#11547 = CARTESIAN_POINT ( 'NONE',  ( -16.84014894278200458, 499.1198905683720000, 11.84573899990672530 ) ) ;
#11548 = CARTESIAN_POINT ( 'NONE',  ( -48.68588794268870856, 356.9323905601784759, -3.978247347593158345 ) ) ;
#11549 = CARTESIAN_POINT ( 'NONE',  ( 65.85920792673738333, 160.1716627696692683, 40.00000000000000000 ) ) ;
#11550 = VERTEX_POINT ( 'NONE', #20526 ) ;
#11551 = CARTESIAN_POINT ( 'NONE',  ( -35.09675569278795848, 463.4948905683720000, -15.47720386886985544 ) ) ;
#11552 = FACE_OUTER_BOUND ( 'NONE', #874, .T. ) ;
#11553 = CARTESIAN_POINT ( 'NONE',  ( -42.88789093042842637, 272.9323905683720568, -9.489475012073736337 ) ) ;
#11554 = EDGE_LOOP ( 'NONE', ( #20499, #12077, #14514, #2459, #12648, #7991 ) ) ;
#11555 = CARTESIAN_POINT ( 'NONE',  ( -42.82802356641964536, 228.4948905601784759, 14.14213562373094923 ) ) ;
#11556 = EDGE_CURVE ( 'NONE', #10309, #9092, #16095, .T. ) ;
#11557 = CARTESIAN_POINT ( 'NONE',  ( -19.19641293061497223, 281.9323905683720568, -14.20200298773971603 ) ) ;
#11558 = CARTESIAN_POINT ( 'NONE',  ( -45.43829269268869808, 265.6823905683720568, 3.332260488124734632 ) ) ;
#11559 = CARTESIAN_POINT ( 'NONE',  ( -24.70764059509553334, 244.8073905765656377, 19.99999999999998934 ) ) ;
#11560 = CYLINDRICAL_SURFACE ( 'NONE', #14862, 9.999999999999994671 ) ;
#11561 = FACE_OUTER_BOUND ( 'NONE', #13075, .T. ) ;
#11562 = CARTESIAN_POINT ( 'NONE',  ( -45.43829269268869098, 264.1823905683720000, 3.332260488124734632 ) ) ;
#11563 = CARTESIAN_POINT ( 'NONE',  ( -40.53162694259543741, 376.6198905683720568, 11.84573899990672885 ) ) ;
#11564 = CARTESIAN_POINT ( 'NONE',  ( -43.68588794268869435, 200.1437886375728965, 2.403080215999224424E-15 ) ) ;
#11565 = CARTESIAN_POINT ( 'NONE',  ( 0.000000000000000000, 7.511572993685794170E-16, -6.499999999999999112 ) ) ;
#11566 = DIRECTION ( 'NONE',  ( 1.000000000000000000, 0.000000000000000000, 0.000000000000000000 ) ) ;
#11567 = CARTESIAN_POINT ( 'NONE',  ( -13.20868407381886733, 428.2448905683720568, 6.410867750099229490 ) ) ;
#11568 = DIRECTION ( 'NONE',  ( 0.3512089204514979301, 0.000000000000000000, -0.9362971185447991340 ) ) ;
#11569 = ORIENTED_EDGE ( 'NONE', *, *, #6378, .F. ) ;
#11570 = CARTESIAN_POINT ( 'NONE',  ( -48.68588794268871567, 427.5573905601784759, 3.978247347593168115 ) ) ;
#11571 = ORIENTED_EDGE ( 'NONE', *, *, #16439, .T. ) ;
#11572 = VERTEX_POINT ( 'NONE', #10878 ) ;
#11573 = VERTEX_POINT ( 'NONE', #9043 ) ;
#11574 = CARTESIAN_POINT ( 'NONE',  ( -42.82802356641965247, 205.4732429224858379, -5.000000000000002665 ) ) ;
#11575 = CARTESIAN_POINT ( 'NONE',  ( -42.82802356641965247, 298.4948905601784759, 14.14213562373094923 ) ) ;
#11576 = FACE_OUTER_BOUND ( 'NONE', #4048, .T. ) ;
#11577 = CARTESIAN_POINT ( 'NONE',  ( -11.93348319268872260, 350.6823905683719431, -3.332260488124732856 ) ) ;
#11578 = VERTEX_POINT ( 'NONE', #18997 ) ;
#11579 = CARTESIAN_POINT ( 'NONE',  ( -8.685887942688738761, 486.6823905765656946, 3.978247347593161010 ) ) ;
#11580 = CARTESIAN_POINT ( 'NONE',  ( -35.09675569278794427, 371.9948905683720568, -15.47720386886985544 ) ) ;
#11581 = DIRECTION ( 'NONE',  ( -1.000000000000000000, 0.000000000000000000, 0.000000000000000000 ) ) ;
#11582 = CARTESIAN_POINT ( 'NONE',  ( -44.16309181155857289, 394.4948905683720000, 6.410867750099241924 ) ) ;
#11583 = CARTESIAN_POINT ( 'NONE',  ( -10.20829729246297823, 297.6198905765656377, -7.653668647301794969 ) ) ;
#11584 = CARTESIAN_POINT ( 'NONE',  ( -8.685887942688728103, 422.2448905601784759, -2.449293598294705724E-15 ) ) ;
#11585 = CARTESIAN_POINT ( 'NONE',  ( -32.01814843081344009, 291.6823905683720568, -16.75240474999999307 ) ) ;
#11586 = FACE_OUTER_BOUND ( 'NONE', #10922, .T. ) ;
#11587 = CARTESIAN_POINT ( 'NONE',  ( -42.88789093042844058, 436.3073905683720568, 9.489475012073736337 ) ) ;
#11588 = CARTESIAN_POINT ( 'NONE',  ( -10.20829729246297646, 282.8698905601784759, -7.653668647301794969 ) ) ;
#11589 = CARTESIAN_POINT ( 'NONE',  ( -40.01497788969914637, 498.8073905601784759, 16.95518130045146776 ) ) ;
#11590 = DIRECTION ( 'NONE',  ( -0.5877852522924731371, -7.005166667826997985E-17, 0.8090169943749475623 ) ) ;
#11591 = UNCERTAINTY_MEASURE_WITH_UNIT (LENGTH_MEASURE( 1.000000000000000082E-05 ), #14527, 'distance_accuracy_value', 'NONE');
#11592 = DIRECTION ( 'NONE',  ( 0.000000000000000000, 1.000000000000000000, 0.000000000000000000 ) ) ;
#11593 = EDGE_CURVE ( 'NONE', #16560, #5985, #13836, .T. ) ;
#11594 = CARTESIAN_POINT ( 'NONE',  ( -38.17536295476244845, 346.9323905683720568, 14.20200298773971781 ) ) ;
#11595 = CARTESIAN_POINT ( 'NONE',  ( -42.88789093042844769, 474.8073905683720000, 9.489475012073736337 ) ) ;
#11596 = EDGE_CURVE ( 'NONE', #11572, #6694, #5708, .T. ) ;
#11597 = ORIENTED_EDGE ( 'NONE', *, *, #15273, .T. ) ;
#11598 = ADVANCED_FACE ( 'NONE', ( #6221 ), #6428, .F. ) ;
#11599 = CARTESIAN_POINT ( 'NONE',  ( -24.70764059509556532, 480.0573905601784759, 19.99999999999998934 ) ) ;
#11600 = CARTESIAN_POINT ( 'NONE',  ( -28.68588794268870856, 311.3698905683720568, -16.75240474999999307 ) ) ;
#11601 = ADVANCED_FACE ( 'NONE', ( #12728 ), #21370, .T. ) ;
#11602 = CARTESIAN_POINT ( 'NONE',  ( 171.3141120573112630, 610.7448905601785327, 0.000000000000000000 ) ) ;
#11603 = VERTEX_POINT ( 'NONE', #1585 ) ;
#11604 = CARTESIAN_POINT ( 'NONE',  ( -49.57497958038186425, 230.5765313837437418, 60.00000000000000000 ) ) ;
#11605 = CARTESIAN_POINT ( 'NONE',  ( -45.43829269268871940, 395.0573905683719431, -3.332260488124726638 ) ) ;
#11606 = DIRECTION ( 'NONE',  ( 0.000000000000000000, -0.000000000000000000, 1.000000000000000000 ) ) ;
#11607 = CARTESIAN_POINT ( 'NONE',  ( -28.68588794268871922, 426.3698905683720568, 16.75240474999999307 ) ) ;
#11608 = CARTESIAN_POINT ( 'NONE',  ( -32.01814843081345430, 451.6823905683720568, -16.75240474999999307 ) ) ;
#11609 = CARTESIAN_POINT ( 'NONE',  ( -45.64106924314018698, 398.1823905601785327, 11.32908994701042538 ) ) ;
#11610 = EDGE_CURVE ( 'NONE', #18327, #10139, #19633, .T. ) ;
#11611 = CARTESIAN_POINT ( 'NONE',  ( -11.73070664223725146, 367.9323905765655809, -11.32908994701042715 ) ) ;
#11612 = CARTESIAN_POINT ( 'NONE',  ( -22.26996532928915329, 45.30456360475645283, 49.18697961254023454 ) ) ;
#11613 = LINE ( 'NONE', #4691, #613 ) ;
#11614 = CARTESIAN_POINT ( 'NONE',  ( 28.16023193154655502, 323.8848358243226357, 20.00000000000000355 ) ) ;
#11615 = LINE ( 'NONE', #3710, #20751 ) ;
#11616 = CARTESIAN_POINT ( 'NONE',  ( -14.48388495494901385, 489.4323905683720568, 9.489475012073732785 ) ) ;
#11617 = PLANE ( 'NONE',  #10239 ) ;
#11618 = CARTESIAN_POINT ( 'NONE',  ( -42.82802356641967378, 465.9948905601784759, -14.14213562373094746 ) ) ;
#11619 = CARTESIAN_POINT ( 'NONE',  ( -48.68588794268872988, 517.2448905601785327, 0.000000000000000000 ) ) ;
#11620 = VECTOR ( 'NONE', #19493, 1000.000000000000000 ) ;
#11621 = CARTESIAN_POINT ( 'NONE',  ( -28.68588794268871567, 397.8698905683720000, 16.75240474999999307 ) ) ;
#11622 = DIRECTION ( 'NONE',  ( -0.000000000000000000, 1.000000000000000000, -0.000000000000000000 ) ) ;
#11623 = CARTESIAN_POINT ( 'NONE',  ( -11.93348319268870661, 230.6823905683720284, -3.332260488124732856 ) ) ;
#11624 = CARTESIAN_POINT ( 'NONE',  ( -42.88789093042843348, 364.8073905683720568, 9.489475012073736337 ) ) ;
#11625 = CIRCLE ( 'NONE', #16126, 6.500000000000000888 ) ;
#11626 = ORIENTED_EDGE ( 'NONE', *, *, #3816, .F. ) ;
#11627 = CARTESIAN_POINT ( 'NONE',  ( -16.84014894278201169, 520.1198905683720568, -11.84573899990672707 ) ) ;
#11628 = ORIENTED_EDGE ( 'NONE', *, *, #3009, .F. ) ;
#11629 = CARTESIAN_POINT ( 'NONE',  ( -19.19641293061499354, 451.9323905683720568, -14.20200298773971603 ) ) ;
#11630 = CARTESIAN_POINT ( 'NONE',  ( -25.35362745456401257, 531.0573905683720568, -16.75240474999999307 ) ) ;
#11631 = DIRECTION ( 'NONE',  ( -0.4627175328665442677, 0.000000000000000000, 0.8865057725575725689 ) ) ;
#11632 = CARTESIAN_POINT ( 'NONE',  ( -32.66413529028187668, 429.4323905601785896, 19.99999999999999289 ) ) ;
#11633 = CARTESIAN_POINT ( 'NONE',  ( -11.93348319268873503, 478.5573905683721136, 3.332260488124728415 ) ) ;
#11634 = ORIENTED_EDGE ( 'NONE', *, *, #16104, .F. ) ;
#11635 = CARTESIAN_POINT ( 'NONE',  ( -16.84014894278200458, 497.6198905683720000, 11.84573899990672530 ) ) ;
#11636 = CARTESIAN_POINT ( 'NONE',  ( -13.14633856003217360, 49.83395320290721031, -47.10416470750529783 ) ) ;
#11637 = AXIS2_PLACEMENT_3D ( 'NONE', #3719, #4139, #703 ) ;
#11638 = CARTESIAN_POINT ( 'NONE',  ( -36.33955658999052218, 450.1198905765655809, -18.47759065022572855 ) ) ;
#11639 = LINE ( 'NONE', #195, #11697 ) ;
#11640 = CARTESIAN_POINT ( 'NONE',  ( -24.70764059509554755, 249.1823905765656093, -19.99999999999999289 ) ) ;
#11641 = PLANE ( 'NONE',  #19436 ) ;
#11642 = CARTESIAN_POINT ( 'NONE',  ( 0.000000000000000000, 4.898587196589412829E-16, -4.000000000000000000 ) ) ;
#11643 = VECTOR ( 'NONE', #18764, 1000.000000000000000 ) ;
#11644 = CARTESIAN_POINT ( 'NONE',  ( -28.68588794268874054, 573.2448905601785327, 0.000000000000000000 ) ) ;
#11645 = CARTESIAN_POINT ( 'NONE',  ( -47.16347859291445843, 492.6198905765656377, 7.653668647301805628 ) ) ;
#11646 = CARTESIAN_POINT ( 'NONE',  ( -40.53162694259543031, 294.1198905683720568, -11.84573899990672707 ) ) ;
#11647 = CARTESIAN_POINT ( 'NONE',  ( -48.68588794268872988, 527.2448905601785327, 0.000000000000000000 ) ) ;
#11648 = CARTESIAN_POINT ( 'NONE',  ( -10.20829729246297646, 271.6198905601784759, 7.653668647301790529 ) ) ;
#11649 = CARTESIAN_POINT ( 'NONE',  ( -42.82802356641966668, 413.2448905765655809, 14.14213562373094923 ) ) ;
#11650 = CARTESIAN_POINT ( 'NONE',  ( -44.16309181155856578, 294.7448905683720568, -6.410867750099231266 ) ) ;
#11651 = EDGE_CURVE ( 'NONE', #20871, #11812, #5837, .T. ) ;
#11652 = AXIS2_PLACEMENT_3D ( 'NONE', #5997, #17785, #12710 ) ;
#11653 = CARTESIAN_POINT ( 'NONE',  ( -40.01497788969916058, 535.6823905601784190, -16.95518130045146421 ) ) ;
#11654 = CARTESIAN_POINT ( 'NONE',  ( -35.09675569278796559, 513.4948905683720568, -15.47720386886985544 ) ) ;
#11655 = VECTOR ( 'NONE', #12337, 1000.000000000000227 ) ;
#11656 = EDGE_LOOP ( 'NONE', ( #9622, #14173, #8532 ) ) ;
#11657 = CARTESIAN_POINT ( 'NONE',  ( -28.68588794268872988, 472.8698905683720568, -16.75240474999999307 ) ) ;
#11658 = EDGE_CURVE ( 'NONE', #13368, #10871, #3312, .T. ) ;
#11659 = LINE ( 'NONE', #15138, #2108 ) ;
#11660 = CARTESIAN_POINT ( 'NONE',  ( -22.27502019258947641, 270.7448905683720568, -15.47720386886985544 ) ) ;
#11661 = EDGE_LOOP ( 'NONE', ( #4603, #234, #9647, #9542, #4922 ) ) ;
#11662 =( BOUNDED_CURVE ( )  B_SPLINE_CURVE ( 2, ( #6882, #8826, #630, #1939, #8505, #10334, #5364, #314, #18460, #3649, #11968, #18565, #16957, #7196, #2138, #528, #13818 ),
 .UNSPECIFIED., .F., .T. ) 
 B_SPLINE_CURVE_WITH_KNOTS ( ( 3, 2, 2, 2, 2, 2, 2, 2, 3 ),
 ( 0.8281250000000002220, 0.8300781250000002220, 0.8320312500000002220, 0.8339843750000002220, 0.8359375000000002220, 0.8378906250000002220, 0.8398437500000002220, 0.8417968750000002220, 0.8437500000000002220 ),
 .UNSPECIFIED. ) 
 CURVE ( )  GEOMETRIC_REPRESENTATION_ITEM ( )  RATIONAL_B_SPLINE_CURVE ( ( 0.9999999999999977796, 0.9807852804032326510, 1.000000000000000000, 0.9807852804032304306, 1.000000000000000000, 0.9807852804032304306, 1.000000000000000000, 0.9807852804032304306, 1.000000000000000000, 0.9807852804032304306, 1.000000000000000000, 0.9807852804032304306, 1.000000000000000000, 0.9807852804032304306, 1.000000000000000000, 0.9807852804032282101, 1.000000000000002220 ) ) 
 REPRESENTATION_ITEM ( '' )  );
#11663 = FACE_OUTER_BOUND ( 'NONE', #17036, .T. ) ;
#11664 = CARTESIAN_POINT ( 'NONE',  ( -13.20868407381884779, 269.7448905683720568, 6.410867750099229490 ) ) ;
#11665 = CARTESIAN_POINT ( 'NONE',  ( -38.17536295476244135, 253.8073905683720284, -14.20200298773971426 ) ) ;
#11666 = CARTESIAN_POINT ( 'NONE',  ( -28.68588794268869790, 244.4948905765655809, 19.99999999999999289 ) ) ;
#11667 = DIRECTION ( 'NONE',  ( 1.191790137725560488E-16, -1.000000000000000000, -0.000000000000000000 ) ) ;
#11668 = CARTESIAN_POINT ( 'NONE',  ( -36.33955658999050087, 229.1198905601785043, 18.47759065022572500 ) ) ;
#11669 = LINE ( 'NONE', #20608, #2689 ) ;
#11670 = CARTESIAN_POINT ( 'NONE',  ( -16.84014894278197971, 270.1198905683720568, -11.84573899990672707 ) ) ;
#11671 = CARTESIAN_POINT ( 'NONE',  ( -42.88789093042843348, 354.4323905683720568, -9.489475012073736337 ) ) ;
#11672 = CARTESIAN_POINT ( 'NONE',  ( -48.68588794268870146, 277.2448905601784759, 0.000000000000000000 ) ) ;
#11673 = CARTESIAN_POINT ( 'NONE',  ( 20.42502041961813930, 230.5765313837437418, 60.00000000000000000 ) ) ;
#11674 = ADVANCED_FACE ( 'NONE', ( #18116 ), #14470, .T. ) ;
#11675 = CARTESIAN_POINT ( 'NONE',  ( -28.68588794268872277, 431.3698905683720000, -16.75240474999999307 ) ) ;
#11676 = CARTESIAN_POINT ( 'NONE',  ( -24.70764059509555466, 339.1823905765656377, -19.99999999999999289 ) ) ;
#11677 = ORIENTED_EDGE ( 'NONE', *, *, #5421, .T. ) ;
#11678 = CARTESIAN_POINT ( 'NONE',  ( -8.685887942688728103, 421.9323905601785327, 3.978247347593161010 ) ) ;
#11679 = VERTEX_POINT ( 'NONE', #16514 ) ;
#11680 = DIRECTION ( 'NONE',  ( 0.000000000000000000, 0.000000000000000000, 1.000000000000000000 ) ) ;
#11681 = VERTEX_POINT ( 'NONE', #8264 ) ;
#11682 = VERTEX_POINT ( 'NONE', #20947 ) ;
#11683 = CARTESIAN_POINT ( 'NONE',  ( -16.84014894278200813, 529.1198905683720568, 11.84573899990672530 ) ) ;
#11684 = CARTESIAN_POINT ( 'NONE',  ( -24.70764059509554045, 310.0573905601784759, 19.99999999999998934 ) ) ;
#11685 = CARTESIAN_POINT ( 'NONE',  ( -2.085632741019731137E-15, 610.7448905601785327, 0.000000000000000000 ) ) ;
#11686 = CARTESIAN_POINT ( 'NONE',  ( -11.93348319268872260, 340.6823905683720000, -3.332260488124732856 ) ) ;
#11687 = EDGE_LOOP ( 'NONE', ( #18115, #7442, #20569, #8802, #14176, #7277 ) ) ;
#11688 = CARTESIAN_POINT ( 'NONE',  ( -8.685887942688736985, 476.6823905765656377, 3.978247347593161010 ) ) ;
#11689 = CARTESIAN_POINT ( 'NONE',  ( -40.53162694259543741, 372.6198905683720000, -11.84573899990672707 ) ) ;
#11690 = CARTESIAN_POINT ( 'NONE',  ( -44.16309181155857289, 363.2448905683720000, -6.410867750099231266 ) ) ;
#11691 = ADVANCED_FACE ( 'NONE', ( #9474 ), #13044, .F. ) ;
#11692 = CARTESIAN_POINT ( 'NONE',  ( -21.03221929538691626, 298.8698905765656377, -18.47759065022572855 ) ) ;
#11693 = CARTESIAN_POINT ( 'NONE',  ( 52.94681837068318941, 78.74778544605769071, 94.99999999999994316 ) ) ;
#11694 = CARTESIAN_POINT ( 'NONE',  ( -35.09675569278793716, 265.7448905683720000, 15.47720386886985366 ) ) ;
#11695 = DIRECTION ( 'NONE',  ( 0.000000000000000000, 0.000000000000000000, 1.000000000000000000 ) ) ;
#11696 = CARTESIAN_POINT ( 'NONE',  ( -13.20868407381887089, 440.9948905683720568, -6.410867750099233042 ) ) ;
#11697 = VECTOR ( 'NONE', #19750, 1000.000000000000000 ) ;
#11698 = DIRECTION ( 'NONE',  ( 0.000000000000000000, 0.000000000000000000, -1.000000000000000000 ) ) ;
#11699 = CARTESIAN_POINT ( 'NONE',  ( -45.64106924314020119, 516.3073905601785327, -11.32908994701042538 ) ) ;
#11700 = CARTESIAN_POINT ( 'NONE',  ( -48.68588794268870146, 287.2448905601784759, 0.000000000000000000 ) ) ;
#11701 = EDGE_CURVE ( 'NONE', #1447, #18698, #1082, .T. ) ;
#11702 = CARTESIAN_POINT ( 'NONE',  ( -32.01814843081344719, 333.1823905683720000, -16.75240474999999307 ) ) ;
#11703 = CARTESIAN_POINT ( 'NONE',  ( -11.93348319268873681, 488.8698905683720568, -2.051577885510841163E-15 ) ) ;
#11704 = VERTEX_POINT ( 'NONE', #17802 ) ;
#11705 = CARTESIAN_POINT ( 'NONE',  ( -32.66413529028189089, 479.4323905601785327, 19.99999999999999289 ) ) ;
#11706 = CARTESIAN_POINT ( 'NONE',  ( -19.19641293061497933, 300.4323905683721136, -14.20200298773971603 ) ) ;
#11707 = CARTESIAN_POINT ( 'NONE',  ( 18.20947592957834260, 600.7448905601785327, -168.5995991907681173 ) ) ;
#11708 = ORIENTED_EDGE ( 'NONE', *, *, #15407, .T. ) ;
#11709 = CARTESIAN_POINT ( 'NONE',  ( 40.42502041961814996, 180.1716627696692967, -40.00000000000000000 ) ) ;
#11710 = CIRCLE ( 'NONE', #11361, 50.00000000000000000 ) ;
#11711 = CARTESIAN_POINT ( 'NONE',  ( -14.48388495494900674, 399.4323905683720568, 9.489475012073731008 ) ) ;
#11712 = CARTESIAN_POINT ( 'NONE',  ( -40.01497788969913927, 443.5573905765656377, 16.95518130045146776 ) ) ;
#11713 = FACE_OUTER_BOUND ( 'NONE', #7222, .T. ) ;
#11714 = CARTESIAN_POINT ( 'NONE',  ( -11.93348319268872970, 428.8698905683720568, -2.051577885510841163E-15 ) ) ;
#11715 = CARTESIAN_POINT ( 'NONE',  ( -19.19641293061497223, 251.9323905683720284, -14.20200298773971603 ) ) ;
#11716 = CARTESIAN_POINT ( 'NONE',  ( -25.35362745456399125, 436.6823905683720568, 16.75240474999998952 ) ) ;
#11717 = APPLICATION_PROTOCOL_DEFINITION ( 'draft international standard', 'automotive_design', 1998, #14281 ) ;
#11718 = CARTESIAN_POINT ( 'NONE',  ( -47.16347859291445133, 397.8698905601784759, 7.653668647301805628 ) ) ;
#11719 = CARTESIAN_POINT ( 'NONE',  ( -17.35679799567829917, 368.5573905765655809, -16.95518130045146421 ) ) ;
#11720 = DIRECTION ( 'NONE',  ( 0.000000000000000000, 0.000000000000000000, -1.000000000000000000 ) ) ;
#11721 = CARTESIAN_POINT ( 'NONE',  ( -8.685887942688548691, 387.3073905765655809, -3.978247347592740013 ) ) ;
#11722 = CARTESIAN_POINT ( 'NONE',  ( -28.68588794268871212, 331.3698905683720000, -16.75240474999999307 ) ) ;
#11723 = DIRECTION ( 'NONE',  ( 1.000000000000000000, 0.000000000000000000, 0.000000000000000000 ) ) ;
#11724 = CARTESIAN_POINT ( 'NONE',  ( -44.16309181155857999, 505.9948905683720000, 6.410867750099241924 ) ) ;
#11725 = DIRECTION ( 'NONE',  ( -1.191790137725560488E-16, 1.000000000000000000, -0.000000000000000000 ) ) ;
#11726 = CARTESIAN_POINT ( 'NONE',  ( -47.16347859291445843, 466.6198905601784759, -7.653668647301793193 ) ) ;
#11727 = CARTESIAN_POINT ( 'NONE',  ( -43.31958977256851995, 208.9114094701607485, 3.303159798271270819 ) ) ;
#11728 = VECTOR ( 'NONE', #9401, 1000.000000000000000 ) ;
#11729 = CARTESIAN_POINT ( 'NONE',  ( -45.43829269268871229, 415.0573905683721136, -3.332260488124726194 ) ) ;
#11730 = LINE ( 'NONE', #5021, #16138 ) ;
#11731 = EDGE_CURVE ( 'NONE', #13900, #2082, #2992, .T. ) ;
#11732 = CARTESIAN_POINT ( 'NONE',  ( -32.01814843081343298, 237.5573905683720568, 16.75240474999999307 ) ) ;
#11733 = CARTESIAN_POINT ( 'NONE',  ( -40.53162694259543741, 365.1198905683720000, 11.84573899990672885 ) ) ;
#11734 = EDGE_CURVE ( 'NONE', #13236, #10338, #13312, .T. ) ;
#11735 = EDGE_LOOP ( 'NONE', ( #7099, #11455 ) ) ;
#11736 = CARTESIAN_POINT ( 'NONE',  ( -11.93348319268874036, 519.1823905683719431, -3.332260488124732856 ) ) ;
#11737 = ORIENTED_EDGE ( 'NONE', *, *, #2481, .F. ) ;
#11738 = CARTESIAN_POINT ( 'NONE',  ( -25.35362745456399125, 438.1823905683720000, 16.75240474999998952 ) ) ;
#11739 = CARTESIAN_POINT ( 'NONE',  ( -38.17536295476247687, 522.3073905683721705, -14.20200298773971426 ) ) ;
#11740 = ORIENTED_EDGE ( 'NONE', *, *, #6009, .T. ) ;
#11741 = CYLINDRICAL_SURFACE ( 'NONE', #10022, 19.99999999999999645 ) ;
#11742 = CARTESIAN_POINT ( 'NONE',  ( -44.16309181155858710, 483.2448905683720000, -6.410867750099231266 ) ) ;
#11743 = ORIENTED_EDGE ( 'NONE', *, *, #6430, .F. ) ;
#11744 = CARTESIAN_POINT ( 'NONE',  ( -38.17536295476246977, 515.4323905683720568, 14.20200298773971781 ) ) ;
#11745 = CARTESIAN_POINT ( 'NONE',  ( -25.36211449377851679, 45.71545155958810369, -49.49192749095595190 ) ) ;
#11746 = CARTESIAN_POINT ( 'NONE',  ( -36.33955658999052218, 413.8698905765655809, 18.47759065022572500 ) ) ;
#11747 = CARTESIAN_POINT ( 'NONE',  ( -48.68588794268852382, 251.6823905765656093, -3.978247347593583783 ) ) ;
#11748 = CARTESIAN_POINT ( 'NONE',  ( 0.000000000000000000, 0.000000000000000000, 0.000000000000000000 ) ) ;
#11749 = CARTESIAN_POINT ( 'NONE',  ( -42.82802356641964536, 205.1437886375728965, -5.000000000000001776 ) ) ;
#11750 = DIRECTION ( 'NONE',  ( -0.000000000000000000, 0.000000000000000000, 1.000000000000000000 ) ) ;
#11751 = CYLINDRICAL_SURFACE ( 'NONE', #2851, 9.999999999999994671 ) ;
#11752 = CARTESIAN_POINT ( 'NONE',  ( -43.15146482487497792, 202.0901544311013538, -3.972812079771461224 ) ) ;
#11753 = CARTESIAN_POINT ( 'NONE',  ( -16.84014894278197971, 289.1198905683720568, 11.84573899990672530 ) ) ;
#11754 = FACE_BOUND ( 'NONE', #17947, .T. ) ;
#11755 = CARTESIAN_POINT ( 'NONE',  ( -48.68588794268870146, 277.2448905601784759, 0.000000000000000000 ) ) ;
#11756 = CARTESIAN_POINT ( 'NONE',  ( -33.38097863509928942, 53.57231333527381878, -49.37834231071079927 ) ) ;
#11757 = CARTESIAN_POINT ( 'NONE',  ( -11.93348319268871371, 280.6823905683720000, -3.332260488124732856 ) ) ;
#11758 = VERTEX_POINT ( 'NONE', #8486 ) ;
#11759 = DIRECTION ( 'NONE',  ( 0.000000000000000000, -1.000000000000000000, 0.000000000000000000 ) ) ;
#11760 = CARTESIAN_POINT ( 'NONE',  ( -19.19641293061500065, 511.9323905683721705, -14.20200298773971603 ) ) ;
#11761 = CIRCLE ( 'NONE', #19707, 10.00000000000000888 ) ;
#11762 = ORIENTED_EDGE ( 'NONE', *, *, #8416, .T. ) ;
#11763 = CARTESIAN_POINT ( 'NONE',  ( -13.20868407381887266, 460.9948905683720000, -6.410867750099233042 ) ) ;
#11764 = CARTESIAN_POINT ( 'NONE',  ( 20.42502041961813575, 271.1055109169419666, -20.00000000000000355 ) ) ;
#11765 = CARTESIAN_POINT ( 'NONE',  ( -25.35362745456396638, 256.6823905683720000, 16.75240474999998952 ) ) ;
#11766 = VERTEX_POINT ( 'NONE', #3628 ) ;
#11767 = DIRECTION ( 'NONE',  ( -1.191790137725560488E-16, 1.000000000000000000, -0.000000000000000000 ) ) ;
#11768 = CARTESIAN_POINT ( 'NONE',  ( -19.19641293061497223, 271.9323905683720568, -14.20200298773971603 ) ) ;
#11769 = CARTESIAN_POINT ( 'NONE',  ( -38.17536295476243424, 246.9323905683720284, 14.20200298773971781 ) ) ;
#11770 = CARTESIAN_POINT ( 'NONE',  ( -36.33955658999049376, 250.1198905765656377, -18.47759065022572855 ) ) ;
#11771 = CARTESIAN_POINT ( 'NONE',  ( -36.33955658999050797, 309.1198905601785327, 18.47759065022572500 ) ) ;
#11772 = CARTESIAN_POINT ( 'NONE',  ( -42.82802356641964536, 228.4948905601784759, 14.14213562373094923 ) ) ;
#11773 = CARTESIAN_POINT ( 'NONE',  ( -16.84014894278197971, 260.1198905683720568, -11.84573899990672707 ) ) ;
#11774 = CARTESIAN_POINT ( 'NONE',  ( -19.19641293061498644, 361.9323905683721136, -14.20200298773971603 ) ) ;
#11775 = CARTESIAN_POINT ( 'NONE',  ( -36.33955658999052218, 505.3698905601784190, -18.47759065022572855 ) ) ;
#11776 = DIRECTION ( 'NONE',  ( -0.000000000000000000, 0.000000000000000000, 1.000000000000000000 ) ) ;
#11777 = ADVANCED_FACE ( 'NONE', ( #3419 ), #11741, .T. ) ;
#11778 = CARTESIAN_POINT ( 'NONE',  ( -25.35362745456399480, 401.0573905683720000, -16.75240474999999307 ) ) ;
#11779 = CARTESIAN_POINT ( 'NONE',  ( -8.685887942688720997, 336.9948905765656377, -2.449293598294705724E-15 ) ) ;
#11780 = ORIENTED_EDGE ( 'NONE', *, *, #18960, .T. ) ;
#11781 =( BOUNDED_CURVE ( )  B_SPLINE_CURVE ( 2, ( #19142, #7550, #20764, #19242, #18911, #1195, #4319, #4425, #986, #4213, #10902, #2486, #1092, #14175, #20549, #876, #15690 ),
 .UNSPECIFIED., .F., .T. ) 
 B_SPLINE_CURVE_WITH_KNOTS ( ( 3, 2, 2, 2, 2, 2, 2, 2, 3 ),
 ( 0.7343750000000003331, 0.7363281250000003331, 0.7382812500000002220, 0.7402343750000002220, 0.7421875000000002220, 0.7441406250000002220, 0.7460937500000002220, 0.7480468750000001110, 0.7500000000000001110 ),
 .UNSPECIFIED. ) 
 CURVE ( )  GEOMETRIC_REPRESENTATION_ITEM ( )  RATIONAL_B_SPLINE_CURVE ( ( 0.9999999999999966693, 0.9807852804032337612, 1.000000000000000000, 0.9807852804032304306, 1.000000000000000000, 0.9807852804032304306, 1.000000000000000000, 0.9807852804032304306, 1.000000000000000000, 0.9807852804032304306, 1.000000000000000000, 0.9807852804032304306, 1.000000000000000000, 0.9807852804032304306, 1.000000000000000000, 0.9807852804032293204, 1.000000000000001110 ) ) 
 REPRESENTATION_ITEM ( '' )  );
#11782 = CARTESIAN_POINT ( 'NONE',  ( -8.685887942688726326, 412.2448905601784759, -2.449293598294705724E-15 ) ) ;
#11783 = ORIENTED_EDGE ( 'NONE', *, *, #15335, .T. ) ;
#11784 = ORIENTED_EDGE ( 'NONE', *, *, #910, .T. ) ;
#11785 = ORIENTED_EDGE ( 'NONE', *, *, #20411, .T. ) ;
#11786 = CARTESIAN_POINT ( 'NONE',  ( -16.84014894278201169, 521.6198905683719431, -11.84573899990672707 ) ) ;
#11787 = CARTESIAN_POINT ( 'NONE',  ( -48.68588794268870146, 287.5573905601784759, 3.978247347593168115 ) ) ;
#11788 = CARTESIAN_POINT ( 'NONE',  ( -43.37443857369948574, 209.1166545091122657, -3.053198389463521956 ) ) ;
#11789 = CARTESIAN_POINT ( 'NONE',  ( -45.43829269268870519, 325.6823905683720568, 3.332260488124734632 ) ) ;
#11790 = AXIS2_PLACEMENT_3D ( 'NONE', #6911, #2065, #3777 ) ;
#11791 = CARTESIAN_POINT ( 'NONE',  ( -13.20868407381886023, 359.4948905683720000, -6.410867750099233042 ) ) ;
#11792 = CARTESIAN_POINT ( 'NONE',  ( -22.27502019258948707, 360.7448905683720568, -15.47720386886985544 ) ) ;
#11793 = EDGE_CURVE ( 'NONE', #19427, #11572, #2950, .T. ) ;
#11794 = CARTESIAN_POINT ( 'NONE',  ( -45.64106924314017988, 301.0573905765656377, -11.32908994701042715 ) ) ;
#11795 = DIRECTION ( 'NONE',  ( 0.000000000000000000, -0.000000000000000000, 1.000000000000000000 ) ) ;
#11796 = CARTESIAN_POINT ( 'NONE',  ( -11.93348319268871016, 268.8698905683720000, -2.051577885510841163E-15 ) ) ;
#11797 = CARTESIAN_POINT ( 'NONE',  ( -48.68588794268871567, 437.2448905601785327, 0.000000000000000000 ) ) ;
#11798 = CARTESIAN_POINT ( 'NONE',  ( -40.53162694259544452, 416.6198905683720000, 11.84573899990672885 ) ) ;
#11799 = CARTESIAN_POINT ( 'NONE',  ( -31.66342138406952245, 50.08936347150523005, 120.9234288415484002 ) ) ;
#11800 = CARTESIAN_POINT ( 'NONE',  ( -10.20829729246300310, 512.8698905601785327, -7.653668647301794969 ) ) ;
#11801 = CARTESIAN_POINT ( 'NONE',  ( -21.03221929538690915, 360.3698905601784759, 18.47759065022572500 ) ) ;
#11802 = PRODUCT_DEFINITION_CONTEXT ( 'detailed design', #2389, 'design' ) ;
#11803 = CARTESIAN_POINT ( 'NONE',  ( -28.68588794268871922, 409.7448905601784759, 19.99999999999999289 ) ) ;
#11804 = CARTESIAN_POINT ( 'NONE',  ( -45.43829269268869808, 325.0573905683719431, -3.332260488124726194 ) ) ;
#11805 = CARTESIAN_POINT ( 'NONE',  ( -13.20868407381887266, 478.2448905683720568, 6.410867750099229490 ) ) ;
#11806 = VECTOR ( 'NONE', #7097, 1000.000000000000227 ) ;
#11807 = ORIENTED_EDGE ( 'NONE', *, *, #16643, .T. ) ;
#11808 = AXIS2_PLACEMENT_3D ( 'NONE', #10325, #6767, #3534 ) ;
#11809 = CARTESIAN_POINT ( 'NONE',  ( -36.33955658999052929, 459.1198905601784759, 18.47759065022572500 ) ) ;
#11810 = CARTESIAN_POINT ( 'NONE',  ( -13.20868407381885135, 308.2448905683720000, 6.410867750099229490 ) ) ;
#11811 = EDGE_CURVE ( 'NONE', #10102, #6145, #19356, .T. ) ;
#11812 = VERTEX_POINT ( 'NONE', #2021 ) ;
#11813 = CARTESIAN_POINT ( 'NONE',  ( -14.54375231895776466, 345.7448905765655809, 14.14213562373094568 ) ) ;
#11814 = EDGE_LOOP ( 'NONE', ( #15074, #19243 ) ) ;
#11815 = DIRECTION ( 'NONE',  ( -1.191790137725560488E-16, 1.000000000000000000, -0.000000000000000000 ) ) ;
#11816 = CARTESIAN_POINT ( 'NONE',  ( -14.48388495494900141, 381.3073905683720568, -9.489475012073734561 ) ) ;
#11817 = CARTESIAN_POINT ( 'NONE',  ( -28.68588794268872633, 479.7448905601784759, 19.99999999999999289 ) ) ;
#11818 = CARTESIAN_POINT ( 'NONE',  ( -28.68588794268872277, 333.8848358243226357, 38.00000000000000000 ) ) ;
#11819 = CARTESIAN_POINT ( 'NONE',  ( -13.20868407381886733, 428.2448905683720568, 6.410867750099229490 ) ) ;
#11820 = CARTESIAN_POINT ( 'NONE',  ( -40.53162694259542320, 264.1198905683720568, -11.84573899990672707 ) ) ;
#11821 = CARTESIAN_POINT ( 'NONE',  ( -42.88789093042844058, 432.9323905683719431, -9.489475012073734561 ) ) ;
#11822 = DIRECTION ( 'NONE',  ( 1.000000000000000000, 0.000000000000000000, 0.000000000000000000 ) ) ;
#11823 = CARTESIAN_POINT ( 'NONE',  ( -21.03221929538691271, 400.3698905601785327, 18.47759065022572500 ) ) ;
#11824 = EDGE_CURVE ( 'NONE', #11085, #8097, #8700, .T. ) ;
#11825 = CARTESIAN_POINT ( 'NONE',  ( -21.03221929538690915, 355.1198905765656377, 18.47759065022572500 ) ) ;
#11826 = CARTESIAN_POINT ( 'NONE',  ( -22.30770786884145451, 56.85652257517428865, -152.3753892284480003 ) ) ;
#11827 = DIRECTION ( 'NONE',  ( 1.191790137725560488E-16, -1.000000000000000000, -0.000000000000000000 ) ) ;
#11828 = CARTESIAN_POINT ( 'NONE',  ( -22.27502019258948351, 330.7448905683720568, -15.47720386886985544 ) ) ;
#11829 = LINE ( 'NONE', #19839, #15572 ) ;
#11830 = CARTESIAN_POINT ( 'NONE',  ( -42.88789093042844769, 486.3073905683721136, 9.489475012073736337 ) ) ;
#11831 = CARTESIAN_POINT ( 'NONE',  ( -48.68588794268871567, 431.9948905765656377, 0.000000000000000000 ) ) ;
#11832 = LINE ( 'NONE', #281, #6935 ) ;
#11833 = CARTESIAN_POINT ( 'NONE',  ( -42.82802356641964536, 205.1437886375728965, 5.000000000000001776 ) ) ;
#11834 = CARTESIAN_POINT ( 'NONE',  ( -28.68588794268871922, 392.8698905683720000, -16.75240474999999307 ) ) ;
#11835 = CARTESIAN_POINT ( 'NONE',  ( -24.91082379854346129, 45.60735762703961171, -122.4932255835355051 ) ) ;
#11836 = VECTOR ( 'NONE', #18553, 1000.000000000000000 ) ;
#11837 = CARTESIAN_POINT ( 'NONE',  ( -28.68588794268869790, 237.8698905683720568, 16.75240474999999307 ) ) ;
#11838 = CARTESIAN_POINT ( 'NONE',  ( -44.16309181155857289, 373.2448905683720000, -6.410867750099231266 ) ) ;
#11839 = VERTEX_POINT ( 'NONE', #11947 ) ;
#11840 = CARTESIAN_POINT ( 'NONE',  ( -44.16309181155858710, 514.4948905683720568, 6.410867750099241924 ) ) ;
#11841 = ORIENTED_EDGE ( 'NONE', *, *, #14991, .F. ) ;
#11842 = CARTESIAN_POINT ( 'NONE',  ( -16.84014894278200103, 441.6198905683720568, -11.84573899990672707 ) ) ;
#11843 = CARTESIAN_POINT ( 'NONE',  ( -16.84014894278200813, 527.6198905683719431, 11.84573899990672530 ) ) ;
#11844 = ORIENTED_EDGE ( 'NONE', *, *, #10318, .T. ) ;
#11845 = CARTESIAN_POINT ( 'NONE',  ( -47.16347859291445843, 496.6198905601784759, -7.653668647301793193 ) ) ;
#11846 = CARTESIAN_POINT ( 'NONE',  ( -14.48388495494901562, 489.8073905683720568, -9.489475012073736337 ) ) ;
#11847 = CIRCLE ( 'NONE', #5277, 125.0000000000000000 ) ;
#11848 = VERTEX_POINT ( 'NONE', #13268 ) ;
#11849 = CARTESIAN_POINT ( 'NONE',  ( -16.84014894278200458, 490.1198905683720000, -11.84573899990672707 ) ) ;
#11850 = CARTESIAN_POINT ( 'NONE',  ( -26.35292120220072576, 46.04514432807761892, -49.54662401095963986 ) ) ;
#11851 = CARTESIAN_POINT ( 'NONE',  ( -48.68588794268871567, 422.3073905765656946, 3.978247347593168115 ) ) ;
#11852 = DIRECTION ( 'NONE',  ( 0.000000000000000000, 0.000000000000000000, 1.000000000000000000 ) ) ;
#11853 = CARTESIAN_POINT ( 'NONE',  ( -10.20829729246297291, 247.6198905765656377, -7.653668647301794969 ) ) ;
#11854 = CARTESIAN_POINT ( 'NONE',  ( 0.000000000000000000, 326.0737056351150613, -25.00000000000000000 ) ) ;
#11855 = FACE_OUTER_BOUND ( 'NONE', #11270, .T. ) ;
#11856 = AXIS2_PLACEMENT_3D ( 'NONE', #4409, #15778, #9481 ) ;
#11857 = DIRECTION ( 'NONE',  ( -1.191790137725560488E-16, 1.000000000000000000, -0.000000000000000000 ) ) ;
#11858 = CARTESIAN_POINT ( 'NONE',  ( 5.074999999999999289, 6.500000000000000888, 0.000000000000000000 ) ) ;
#11859 = CARTESIAN_POINT ( 'NONE',  ( -32.01814843081344009, 307.5573905683719431, 16.75240474999999307 ) ) ;
#11860 = CARTESIAN_POINT ( 'NONE',  ( -41.83569717483972994, 135.1716627696692683, 24.99999999999998934 ) ) ;
#11861 = CARTESIAN_POINT ( 'NONE',  ( -44.16309181155857999, 455.9948905683720000, 6.410867750099241924 ) ) ;
#11862 = DIRECTION ( 'NONE',  ( -1.000000000000000000, -0.000000000000000000, -0.000000000000000000 ) ) ;
#11863 = CARTESIAN_POINT ( 'NONE',  ( -40.53162694259543031, 294.1198905683720568, -11.84573899990672707 ) ) ;
#11864 = EDGE_CURVE ( 'NONE', #6799, #5796, #5156, .T. ) ;
#11865 = VECTOR ( 'NONE', #19876, 1000.000000000000000 ) ;
#11866 = ORIENTED_EDGE ( 'NONE', *, *, #1654, .T. ) ;
#11867 = CARTESIAN_POINT ( 'NONE',  ( -36.33955658999052929, 535.3698905601784190, -18.47759065022572855 ) ) ;
#11868 = CARTESIAN_POINT ( 'NONE',  ( -44.16309181155858710, 494.7448905683720000, -6.410867750099231266 ) ) ;
#11869 = EDGE_CURVE ( 'NONE', #7807, #1524, #18856, .T. ) ;
#11870 = CIRCLE ( 'NONE', #13613, 4.000000000000001776 ) ;
#11871 = EDGE_CURVE ( 'NONE', #9392, #5108, #4046, .T. ) ;
#11872 = ORIENTED_EDGE ( 'NONE', *, *, #107, .T. ) ;
#11873 = CARTESIAN_POINT ( 'NONE',  ( -28.68588794268872277, 457.8698905683720000, 16.75240474999999307 ) ) ;
#11874 = CARTESIAN_POINT ( 'NONE',  ( 5.074999999999999289, 5.629165124598847214, -3.250000000000007550 ) ) ;
#11875 = CARTESIAN_POINT ( 'NONE',  ( -35.09675569278793716, 255.7448905683720284, 15.47720386886985366 ) ) ;
#11876 = ORIENTED_EDGE ( 'NONE', *, *, #7494, .T. ) ;
#11877 = CARTESIAN_POINT ( 'NONE',  ( 5.074999999999999289, -7.505553499465148271, 0.000000000000000000 ) ) ;
#11878 = CARTESIAN_POINT ( 'NONE',  ( -45.43829269268869808, 235.6823905683720284, 3.332260488124734632 ) ) ;
#11879 = ADVANCED_FACE ( 'NONE', ( #19083 ), #931, .T. ) ;
#11880 = DIRECTION ( 'NONE',  ( 0.000000000000000000, 0.000000000000000000, -1.000000000000000000 ) ) ;
#11881 = CARTESIAN_POINT ( 'NONE',  ( 88.28695088269886071, 152.5259582928263740, 20.00000000000000355 ) ) ;
#11882 = CARTESIAN_POINT ( 'NONE',  ( -14.48388495494898720, 267.9323905683720568, 9.489475012073732785 ) ) ;
#11883 = VECTOR ( 'NONE', #13345, 1000.000000000000000 ) ;
#11884 = CARTESIAN_POINT ( 'NONE',  ( -25.35362745456398059, 348.1823905683720000, 16.75240474999998952 ) ) ;
#11885 = CARTESIAN_POINT ( 'NONE',  ( -25.35362745456399836, 411.0573905683720568, -16.75240474999999307 ) ) ;
#11886 = FACE_OUTER_BOUND ( 'NONE', #14092, .T. ) ;
#11887 = ORIENTED_EDGE ( 'NONE', *, *, #16114, .T. ) ;
#11888 = CARTESIAN_POINT ( 'NONE',  ( -47.16347859291445133, 407.8698905601784759, 7.653668647301805628 ) ) ;
#11889 = EDGE_LOOP ( 'NONE', ( #8096, #14343, #10604 ) ) ;
#11890 = CARTESIAN_POINT ( 'NONE',  ( 146.1533239063698772, 600.7448905601785327, -7.500000000000000000 ) ) ;
#11891 = ORIENTED_EDGE ( 'NONE', *, *, #13055, .T. ) ;
#11892 = ORIENTED_EDGE ( 'NONE', *, *, #2565, .T. ) ;
#11893 = CARTESIAN_POINT ( 'NONE',  ( -11.93348319268874036, 520.3698905683720568, -2.051577885510841163E-15 ) ) ;
#11894 = CARTESIAN_POINT ( 'NONE',  ( -48.68588794268870146, 286.9323905601785327, -3.978247347593158345 ) ) ;
#11895 = CARTESIAN_POINT ( 'NONE',  ( 0.5805565836007647862, 7.505553499465139389, 2.227827669841787811E-16 ) ) ;
#11896 = CARTESIAN_POINT ( 'NONE',  ( -25.35362745456397704, 318.1823905683720568, 16.75240474999998952 ) ) ;
#11897 = VERTEX_POINT ( 'NONE', #5667 ) ;
#11898 = CARTESIAN_POINT ( 'NONE',  ( -45.43829269268870519, 363.5573905683720568, -3.332260488124726194 ) ) ;
#11899 = CARTESIAN_POINT ( 'NONE',  ( -13.20868407381885845, 358.2448905683720000, 6.410867750099229490 ) ) ;
#11900 = CARTESIAN_POINT ( 'NONE',  ( -48.68588794268870146, 301.6823905765655809, -3.978247347593158345 ) ) ;
#11901 = DIRECTION ( 'NONE',  ( 0.000000000000000000, 1.000000000000000000, 0.000000000000000000 ) ) ;
#11902 = CARTESIAN_POINT ( 'NONE',  ( -45.43829269268869808, 264.1823905683719431, 3.332260488124734632 ) ) ;
#11903 = CARTESIAN_POINT ( 'NONE',  ( 5.299999999999999822, 7.505553499465139389, 0.000000000000000000 ) ) ;
#11904 = CARTESIAN_POINT ( 'NONE',  ( -42.88789093042844058, 414.4323905683721136, -9.489475012073736337 ) ) ;
#11905 = CARTESIAN_POINT ( 'NONE',  ( -29.31767284124665807, 47.65796585322660661, 121.5149936206099284 ) ) ;
#11906 = CARTESIAN_POINT ( 'NONE',  ( -48.68588794268872277, 451.9948905765656377, 0.000000000000000000 ) ) ;
#11907 = CARTESIAN_POINT ( 'NONE',  ( -45.64106924314017277, 302.9323905765656946, 11.32908994701042538 ) ) ;
#11908 = CARTESIAN_POINT ( 'NONE',  ( -36.33955658999052218, 409.1198905601784759, 18.47759065022572500 ) ) ;
#11909 = CARTESIAN_POINT ( 'NONE',  ( -22.27502019258947286, 328.4948905683720568, 15.47720386886985189 ) ) ;
#11910 = CARTESIAN_POINT ( 'NONE',  ( -11.93348319268873503, 468.5573905683720000, 3.332260488124728415 ) ) ;
#11911 = EDGE_LOOP ( 'NONE', ( #6726, #9395, #1288, #16508, #14777, #2269, #15005, #4973 ) ) ;
#11912 = CARTESIAN_POINT ( 'NONE',  ( -28.68588794268872277, 459.7448905601784759, 19.99999999999999289 ) ) ;
#11913 = CARTESIAN_POINT ( 'NONE',  ( -44.16309181155856578, 293.2448905683720000, -6.410867750099231266 ) ) ;
#11914 = ADVANCED_FACE ( 'NONE', ( #18753 ), #2329, .T. ) ;
#11915 = CARTESIAN_POINT ( 'NONE',  ( -10.20829729246298356, 341.6198905601784759, 7.653668647301790529 ) ) ;
#11916 = ORIENTED_EDGE ( 'NONE', *, *, #8627, .F. ) ;
#11917 = DIRECTION ( 'NONE',  ( 1.000000000000000000, 0.000000000000000000, 0.000000000000000000 ) ) ;
#11918 = APPLICATION_CONTEXT ( 'automotive_design' ) ;
#11919 = CARTESIAN_POINT ( 'NONE',  ( -16.84014894278199392, 391.6198905683720568, -11.84573899990672707 ) ) ;
#11920 = CARTESIAN_POINT ( 'NONE',  ( -24.70764059509555821, 444.8073905765655809, 19.99999999999998934 ) ) ;
#11921 = EDGE_CURVE ( 'NONE', #5413, #2137, #11761, .T. ) ;
#11922 = CARTESIAN_POINT ( 'NONE',  ( -48.68588794268887199, 382.3073905765655240, 3.978247347592742678 ) ) ;
#11923 = CARTESIAN_POINT ( 'NONE',  ( -19.19641293061498999, 420.4323905683720000, -14.20200298773971603 ) ) ;
#11924 = CARTESIAN_POINT ( 'NONE',  ( -11.93348319268871016, 270.3698905683720000, -2.051577885510841163E-15 ) ) ;
#11925 = CARTESIAN_POINT ( 'NONE',  ( -16.84014894278199748, 420.1198905683720000, -11.84573899990672707 ) ) ;
#11926 = PRODUCT_CONTEXT ( 'NONE', #16890, 'mechanical' ) ;
#11927 = CARTESIAN_POINT ( 'NONE',  ( -8.685887942688719221, 326.9948905765656377, -2.449293598294705724E-15 ) ) ;
#11928 = CARTESIAN_POINT ( 'NONE',  ( -36.33955658999050797, 370.1198905765656377, -18.47759065022572855 ) ) ;
#11929 = CARTESIAN_POINT ( 'NONE',  ( 20.42502041961813575, 271.1055109169419666, -40.00000000000000000 ) ) ;
#11930 = CARTESIAN_POINT ( 'NONE',  ( -32.01814843081344009, 321.6823905683720568, -16.75240474999999307 ) ) ;
#11931 = LINE ( 'NONE', #8360, #19015 ) ;
#11932 = CARTESIAN_POINT ( 'NONE',  ( -38.17536295476246977, 473.8073905683720000, -14.20200298773971426 ) ) ;
#11933 = CARTESIAN_POINT ( 'NONE',  ( -47.16347859291445133, 432.6198905765656377, 7.653668647301805628 ) ) ;
#11934 = DIRECTION ( 'NONE',  ( 0.000000000000000000, 0.000000000000000000, 1.000000000000000000 ) ) ;
#11935 = DIRECTION ( 'NONE',  ( -0.000000000000000000, -0.000000000000000000, 1.000000000000000000 ) ) ;
#11936 = CARTESIAN_POINT ( 'NONE',  ( -42.88789093042844058, 394.4323905683720000, -9.489475012073736337 ) ) ;
#11937 = LINE ( 'NONE', #10733, #2318 ) ;
#11938 = CARTESIAN_POINT ( 'NONE',  ( -10.20829729246300666, 532.8698905601785327, -7.653668647301794969 ) ) ;
#11939 = CARTESIAN_POINT ( 'NONE',  ( -19.19641293061498288, 357.3073905683720568, 14.20200298773971426 ) ) ;
#11940 = EDGE_CURVE ( 'NONE', #6694, #9649, #16346, .T. ) ;
#11941 = ORIENTED_EDGE ( 'NONE', *, *, #1569, .F. ) ;
#11942 = CARTESIAN_POINT ( 'NONE',  ( -19.19641293061499709, 517.3073905683720568, 14.20200298773971426 ) ) ;
#11943 = VERTEX_POINT ( 'NONE', #15639 ) ;
#11944 = CARTESIAN_POINT ( 'NONE',  ( -45.64106924314018698, 356.3073905601785896, -11.32908994701042715 ) ) ;
#11945 = CARTESIAN_POINT ( 'NONE',  ( -11.93348319268874214, 528.5573905683720568, 3.332260488124728415 ) ) ;
#11946 = ORIENTED_EDGE ( 'NONE', *, *, #18597, .F. ) ;
#11947 = CARTESIAN_POINT ( 'NONE',  ( -22.30770786884143675, 45.31613216062291372, 122.9933582338429687 ) ) ;
#11948 = CARTESIAN_POINT ( 'NONE',  ( -19.19641293061499354, 477.3073905683720568, 14.20200298773971426 ) ) ;
#11949 = VERTEX_POINT ( 'NONE', #7391 ) ;
#11950 = CARTESIAN_POINT ( 'NONE',  ( -44.16309181155857999, 484.4948905683720000, 6.410867750099241924 ) ) ;
#11951 = CARTESIAN_POINT ( 'NONE',  ( -26.84078544385846143, 46.24045653294090386, -49.56718956592591496 ) ) ;
#11952 = CARTESIAN_POINT ( 'NONE',  ( -8.685887942688728103, 417.3073905765656377, -3.978247347593165895 ) ) ;
#11953 = CARTESIAN_POINT ( 'NONE',  ( -8.685887942688868435, 476.6823905765656377, 3.978247347593479866 ) ) ;
#11954 = DIRECTION ( 'NONE',  ( 0.000000000000000000, 0.000000000000000000, 1.000000000000000000 ) ) ;
#11955 = LINE ( 'NONE', #15431, #6671 ) ;
#11956 = DIRECTION ( 'NONE',  ( -1.000000000000000000, 0.000000000000000000, 0.000000000000000000 ) ) ;
#11957 = EDGE_CURVE ( 'NONE', #12829, #7636, #2447, .T. ) ;
#11958 = AXIS2_PLACEMENT_3D ( 'NONE', #3926, #700, #2423 ) ;
#11959 = PLANE ( 'NONE',  #17659 ) ;
#11960 = CARTESIAN_POINT ( 'NONE',  ( -45.43829269268869808, 295.6823905683720000, 3.332260488124734632 ) ) ;
#11961 = AXIS2_PLACEMENT_3D ( 'NONE', #7004, #438, #332 ) ;
#11962 = CARTESIAN_POINT ( 'NONE',  ( -32.66413529028189089, 529.4323905601785327, 19.99999999999999289 ) ) ;
#11963 = CARTESIAN_POINT ( 'NONE',  ( -45.43829269268871229, 445.6823905683720000, 3.332260488124734632 ) ) ;
#11964 = CARTESIAN_POINT ( 'NONE',  ( -32.66413529028187668, 414.1823905765656946, 19.99999999999999289 ) ) ;
#11965 = CARTESIAN_POINT ( 'NONE',  ( -42.88789093042842637, 274.4323905683720568, -9.489475012073736337 ) ) ;
#11966 = ADVANCED_FACE ( 'NONE', ( #15744 ), #7497, .T. ) ;
#11967 = ORIENTED_EDGE ( 'NONE', *, *, #9237, .T. ) ;
#11968 = CARTESIAN_POINT ( 'NONE',  ( -36.33955658999050087, 269.1198905601784759, 18.47759065022572500 ) ) ;
#11969 = CARTESIAN_POINT ( 'NONE',  ( -13.20868407381887621, 499.7448905683720000, 6.410867750099229490 ) ) ;
#11970 = AXIS2_PLACEMENT_3D ( 'NONE', #18956, #12042, #17242 ) ;
#11971 = ORIENTED_EDGE ( 'NONE', *, *, #18440, .T. ) ;
#11972 = CARTESIAN_POINT ( 'NONE',  ( -40.53162694259545162, 466.6198905683720000, 11.84573899990672885 ) ) ;
#11973 = CARTESIAN_POINT ( 'NONE',  ( -28.68588794268872277, 409.4948905765656377, -19.99999999999999289 ) ) ;
#11974 = CARTESIAN_POINT ( 'NONE',  ( -13.20868407381884957, 269.4948905683720000, -6.410867750099233042 ) ) ;
#11975 = ORIENTED_EDGE ( 'NONE', *, *, #21380, .T. ) ;
#11976 = PLANE ( 'NONE',  #11082 ) ;
#11977 = CARTESIAN_POINT ( 'NONE',  ( -28.68588794268870146, 267.8698905683720000, 16.75240474999999307 ) ) ;
#11978 = VECTOR ( 'NONE', #12929, 1000.000000000000000 ) ;
#11979 = CARTESIAN_POINT ( 'NONE',  ( -28.68588794268874054, 573.2448905601785327, 0.000000000000000000 ) ) ;
#11980 = MANIFOLD_SOLID_BREP ( 'HeadFillet', #13145 ) ;
#11981 = CARTESIAN_POINT ( 'NONE',  ( -32.01814843081343298, 253.1823905683720568, -16.75240474999999307 ) ) ;
#11982 = CARTESIAN_POINT ( 'NONE',  ( -45.64106924314018698, 421.0573905765655809, -11.32908994701042538 ) ) ;
#11983 = CARTESIAN_POINT ( 'NONE',  ( -40.01497788969912506, 235.6823905601785043, -16.95518130045146421 ) ) ;
#11984 = CARTESIAN_POINT ( 'NONE',  ( -25.35362745456398059, 271.0573905683720000, -16.75240474999999307 ) ) ;
#11985 = CARTESIAN_POINT ( 'NONE',  ( -16.84014894278198682, 359.1198905683720568, 11.84573899990672530 ) ) ;
#11986 = VECTOR ( 'NONE', #5675, 1000.000000000000000 ) ;
#11987 = DIRECTION ( 'NONE',  ( -1.000000000000000000, -0.000000000000000000, -0.000000000000000000 ) ) ;
#11988 = CIRCLE ( 'NONE', #963, 3.309499999999999886 ) ;
#11989 = CARTESIAN_POINT ( 'NONE',  ( -22.27502019258949062, 400.7448905683720568, -15.47720386886985544 ) ) ;
#11990 = CARTESIAN_POINT ( 'NONE',  ( 60.69669829156632090, 56.85652257517428865, 94.99999999999994316 ) ) ;
#11991 = EDGE_CURVE ( 'NONE', #12371, #13587, #7916, .T. ) ;
#11992 = CARTESIAN_POINT ( 'NONE',  ( -8.685887942688726326, 402.2448905601784759, -2.449293598294705724E-15 ) ) ;
#11993 = EDGE_CURVE ( 'NONE', #18701, #5552, #20819, .T. ) ;
#11994 = ORIENTED_EDGE ( 'NONE', *, *, #5505, .T. ) ;
#11995 = CARTESIAN_POINT ( 'NONE',  ( -14.54375231895776821, 348.2448905765656377, -14.14213562373094746 ) ) ;
#11996 = VERTEX_POINT ( 'NONE', #3180 ) ;
#11997 = VERTEX_POINT ( 'NONE', #16274 ) ;
#11998 = LINE ( 'NONE', #8319, #12866 ) ;
#11999 = CARTESIAN_POINT ( 'NONE',  ( -42.82802356641965247, 288.4948905601785327, 14.14213562373094923 ) ) ;
#12000 = CARTESIAN_POINT ( 'NONE',  ( -17.35679799567829207, 318.5573905765656377, -16.95518130045146421 ) ) ;
#12001 = CARTESIAN_POINT ( 'NONE',  ( -11.93348319268871549, 320.6823905683720000, -3.332260488124732856 ) ) ;
#12002 = AXIS2_PLACEMENT_3D ( 'NONE', #15433, #15039, #10539 ) ;
#12003 = ORIENTED_EDGE ( 'NONE', *, *, #12040, .T. ) ;
#12004 = CARTESIAN_POINT ( 'NONE',  ( -32.01814843081344719, 336.0573905683721136, 16.75240474999999307 ) ) ;
#12005 = CARTESIAN_POINT ( 'NONE',  ( -45.43829269268871229, 363.5573905683720568, -3.332260488124726638 ) ) ;
#12006 = AXIS2_PLACEMENT_3D ( 'NONE', #3453, #11987, #10038 ) ;
#12007 = CARTESIAN_POINT ( 'NONE',  ( -28.68588794268870501, 304.4948905765656377, 19.99999999999999289 ) ) ;
#12008 = DIRECTION ( 'NONE',  ( 1.000000000000000000, 0.000000000000000000, -0.000000000000000000 ) ) ;
#12009 = CARTESIAN_POINT ( 'NONE',  ( -13.20868407381884957, 269.4948905683720000, -6.410867750099233042 ) ) ;
#12010 = CARTESIAN_POINT ( 'NONE',  ( -11.73070664223725856, 466.0573905765656946, 11.32908994701042005 ) ) ;
#12011 = CARTESIAN_POINT ( 'NONE',  ( -35.09675569278795138, 423.4948905683720568, -15.47720386886985544 ) ) ;
#12012 = LINE ( 'NONE', #18709, #15135 ) ;
#12013 = CARTESIAN_POINT ( 'NONE',  ( -24.70764059509556887, 449.1823905765655809, -19.99999999999999289 ) ) ;
#12014 = CARTESIAN_POINT ( 'NONE',  ( -33.84809828339280102, 56.85652257517428865, -152.3753892284480003 ) ) ;
#12015 = CARTESIAN_POINT ( 'NONE',  ( -11.93348319268871904, 330.0573905683720568, 3.332260488124728415 ) ) ;
#12016 = CARTESIAN_POINT ( 'NONE',  ( -42.88789093042844769, 472.9323905683720000, -9.489475012073736337 ) ) ;
#12017 = VERTEX_POINT ( 'NONE', #9653 ) ;
#12018 = CARTESIAN_POINT ( 'NONE',  ( -45.64106924314020119, 458.1823905601784190, 11.32908994701042715 ) ) ;
#12019 = CARTESIAN_POINT ( 'NONE',  ( -45.43829269268869808, 283.5573905683720568, -3.332260488124726194 ) ) ;
#12020 = ORIENTED_EDGE ( 'NONE', *, *, #20293, .T. ) ;
#12021 = ORIENTED_EDGE ( 'NONE', *, *, #1392, .T. ) ;
#12022 = DIRECTION ( 'NONE',  ( -1.000000000000000000, 0.000000000000000000, 0.000000000000000000 ) ) ;
#12023 = CARTESIAN_POINT ( 'NONE',  ( -32.66413529028187668, 339.4323905601784759, 19.99999999999999289 ) ) ;
#12024 = CARTESIAN_POINT ( 'NONE',  ( -44.16309181155856578, 293.2448905683720000, -6.410867750099231266 ) ) ;
#12025 = CARTESIAN_POINT ( 'NONE',  ( -22.27502019258947996, 388.4948905683720000, 15.47720386886985189 ) ) ;
#12026 = CARTESIAN_POINT ( 'NONE',  ( -21.03221929538689494, 230.3698905601784759, 18.47759065022572500 ) ) ;
#12027 = CARTESIAN_POINT ( 'NONE',  ( -47.16347859291446554, 531.3698905765655809, -7.653668647301793193 ) ) ;
#12028 = CARTESIAN_POINT ( 'NONE',  ( -25.35362745456398770, 416.6823905683720568, 16.75240474999998952 ) ) ;
#12029 = CARTESIAN_POINT ( 'NONE',  ( -11.93348319268871016, 260.0573905683720000, 3.332260488124728415 ) ) ;
#12030 = CARTESIAN_POINT ( 'NONE',  ( -13.20868407381886911, 429.4948905683720568, -6.410867750099233042 ) ) ;
#12031 = AXIS2_PLACEMENT_3D ( 'NONE', #9687, #18123, #6437 ) ;
#12032 = CARTESIAN_POINT ( 'NONE',  ( -24.70764059509556176, 359.1823905765655809, -19.99999999999999289 ) ) ;
#12033 = CARTESIAN_POINT ( 'NONE',  ( -8.685887942688534480, 272.5573905601784190, -3.978247347592740013 ) ) ;
#12034 = CARTESIAN_POINT ( 'NONE',  ( -11.93348319268871549, 318.5573905683719431, 3.332260488124728859 ) ) ;
#12035 =( BOUNDED_CURVE ( )  B_SPLINE_CURVE ( 2, ( #5604, #10895, #13838, #2478, #4205, #14168, #17504, #5707, #12211, #15575, #2695, #20645, #5815, #10569, #17405, #761, #19132 ),
 .UNSPECIFIED., .F., .T. ) 
 B_SPLINE_CURVE_WITH_KNOTS ( ( 3, 2, 2, 2, 2, 2, 2, 2, 3 ),
 ( 0.6406250000000002220, 0.6425781250000002220, 0.6445312500000002220, 0.6464843750000002220, 0.6484375000000002220, 0.6503906250000002220, 0.6523437500000002220, 0.6542968750000002220, 0.6562500000000002220 ),
 .UNSPECIFIED. ) 
 CURVE ( )  GEOMETRIC_REPRESENTATION_ITEM ( )  RATIONAL_B_SPLINE_CURVE ( ( 0.9999999999999977796, 0.9807852804032326510, 1.000000000000000000, 0.9807852804032304306, 1.000000000000000000, 0.9807852804032304306, 1.000000000000000000, 0.9807852804032304306, 1.000000000000000000, 0.9807852804032304306, 1.000000000000000000, 0.9807852804032304306, 1.000000000000000000, 0.9807852804032304306, 1.000000000000000000, 0.9807852804032282101, 1.000000000000002220 ) ) 
 REPRESENTATION_ITEM ( '' )  );
#12036 = CARTESIAN_POINT ( 'NONE',  ( -32.01814843081346140, 473.1823905683720000, -16.75240474999999307 ) ) ;
#12037 = LINE ( 'NONE', #7057, #13387 ) ;
#12038 = CARTESIAN_POINT ( 'NONE',  ( 43.53705524234220547, -133.1434774248255906, 96.62835994548002816 ) ) ;
#12039 = CARTESIAN_POINT ( 'NONE',  ( -35.86044580198795018, 223.9104597372275123, 18.66884633871304899 ) ) ;
#12040 = EDGE_CURVE ( 'NONE', #8154, #16087, #11383, .T. ) ;
#12041 = CARTESIAN_POINT ( 'NONE',  ( -14.48388495494900141, 381.3073905683720568, -9.489475012073736337 ) ) ;
#12042 = DIRECTION ( 'NONE',  ( 0.000000000000000000, 1.000000000000000000, -0.000000000000000000 ) ) ;
#12043 = EDGE_CURVE ( 'NONE', #4259, #14411, #2757, .T. ) ;
#12044 = CARTESIAN_POINT ( 'NONE',  ( -42.82802356641968089, 528.4948905601785327, 14.14213562373094923 ) ) ;
#12045 = CARTESIAN_POINT ( 'NONE',  ( -11.93348319268872260, 338.5573905683720568, 3.332260488124728415 ) ) ;
#12046 = CIRCLE ( 'NONE', #2735, 20.00000000000000000 ) ;
#12047 = ORIENTED_EDGE ( 'NONE', *, *, #6260, .F. ) ;
#12048 = CARTESIAN_POINT ( 'NONE',  ( -35.09675569278796559, 521.9948905683720568, -15.47720386886985544 ) ) ;
#12049 = VERTEX_POINT ( 'NONE', #12915 ) ;
#12050 = CARTESIAN_POINT ( 'NONE',  ( -40.01497788969913927, 355.6823905601784759, -16.95518130045146421 ) ) ;
#12051 = CARTESIAN_POINT ( 'NONE',  ( -8.685887942688546914, 377.3073905765656377, -3.978247347592740013 ) ) ;
#12052 = CARTESIAN_POINT ( 'NONE',  ( -10.20829729246297113, 227.6198905765656093, -7.653668647301794969 ) ) ;
#12053 = DIRECTION ( 'NONE',  ( 0.000000000000000000, -1.000000000000000000, 0.000000000000000000 ) ) ;
#12054 = DIRECTION ( 'NONE',  ( 0.3090169943749475068, 0.000000000000000000, 0.9510565162951535312 ) ) ;
#12055 = CARTESIAN_POINT ( 'NONE',  ( -25.35362745456399480, 486.6823905683720568, 16.75240474999998952 ) ) ;
#12056 = VERTEX_POINT ( 'NONE', #11496 ) ;
#12057 = CARTESIAN_POINT ( 'NONE',  ( -32.01814843081345430, 481.6823905683720568, -16.75240474999999307 ) ) ;
#12058 = CARTESIAN_POINT ( 'NONE',  ( -21.74034274139373224, 45.28293352602295130, -49.12345169421191571 ) ) ;
#12059 = CARTESIAN_POINT ( 'NONE',  ( -14.54375231895777354, 415.7448905765655809, 14.14213562373094568 ) ) ;
#12060 = CARTESIAN_POINT ( 'NONE',  ( -8.685887942688715668, 296.9948905765655809, -2.449293598294705724E-15 ) ) ;
#12061 = LINE ( 'NONE', #18550, #8539 ) ;
#12062 = AXIS2_PLACEMENT_3D ( 'NONE', #4985, #1537, #18070 ) ;
#12063 = EDGE_CURVE ( 'NONE', #13749, #12049, #11413, .T. ) ;
#12064 = CARTESIAN_POINT ( 'NONE',  ( -8.685887942688733432, 462.2448905601784759, -2.449293598294705724E-15 ) ) ;
#12065 = CARTESIAN_POINT ( 'NONE',  ( -123.2946569474810161, 30.52886280891152282, 20.57735571454641388 ) ) ;
#12066 = DIRECTION ( 'NONE',  ( -1.374938938973709817E-16, 1.000000000000000000, 0.000000000000000000 ) ) ;
#12067 = CARTESIAN_POINT ( 'NONE',  ( -16.84014894278198327, 301.6198905683720000, -11.84573899990672707 ) ) ;
#12068 = CARTESIAN_POINT ( 'NONE',  ( -21.03221929538693047, 530.3698905601784190, 18.47759065022572500 ) ) ;
#12069 = CARTESIAN_POINT ( 'NONE',  ( -13.20868407381886733, 439.7448905683720000, 6.410867750099229490 ) ) ;
#12070 = CARTESIAN_POINT ( 'NONE',  ( -48.68588794268870856, 331.9948905765656377, 0.000000000000000000 ) ) ;
#12071 = CARTESIAN_POINT ( 'NONE',  ( -16.84014894278197971, 271.6198905683720568, -11.84573899990672707 ) ) ;
#12072 = ORIENTED_EDGE ( 'NONE', *, *, #14335, .T. ) ;
#12073 = CARTESIAN_POINT ( 'NONE',  ( -42.82802356641964536, 205.1437886375728965, 5.000000000000001776 ) ) ;
#12074 = CARTESIAN_POINT ( 'NONE',  ( -13.20868407381887266, 479.7448905683720568, 6.410867750099229490 ) ) ;
#12075 = VECTOR ( 'NONE', #21000, 1000.000000000000000 ) ;
#12076 = ADVANCED_FACE ( 'NONE', ( #8128 ), #16064, .F. ) ;
#12077 = ORIENTED_EDGE ( 'NONE', *, *, #16235, .T. ) ;
#12078 = CARTESIAN_POINT ( 'NONE',  ( -22.27502019258948351, 428.4948905683720568, 15.47720386886985189 ) ) ;
#12079 = CARTESIAN_POINT ( 'NONE',  ( 81.24038404635966515, 56.85652257517428865, 94.99999999999994316 ) ) ;
#12080 = CARTESIAN_POINT ( 'NONE',  ( -35.09675569278793006, 251.9948905683720568, -15.47720386886985544 ) ) ;
#12081 = ORIENTED_EDGE ( 'NONE', *, *, #10365, .T. ) ;
#12082 = CARTESIAN_POINT ( 'NONE',  ( 14.09825962131072785, 230.5765313837437418, 49.99999999999999289 ) ) ;
#12083 = CARTESIAN_POINT ( 'NONE',  ( -32.66413529028189089, 474.1823905765655809, 19.99999999999999289 ) ) ;
#12084 = CARTESIAN_POINT ( 'NONE',  ( 20.42502041961813575, 271.1055109169419666, 20.00000000000000355 ) ) ;
#12085 = MANIFOLD_SOLID_BREP ( 'Cut-Extrude10[2]', #12445 ) ;
#12086 = CARTESIAN_POINT ( 'NONE',  ( -44.16309181155855867, 244.7448905683720000, -6.410867750099231266 ) ) ;
#12087 = ADVANCED_FACE ( 'NONE', ( #6195 ), #12807, .T. ) ;
#12088 = CARTESIAN_POINT ( 'NONE',  ( -45.43829269268873361, 515.3698905683720568, 0.000000000000000000 ) ) ;
#12089 = CARTESIAN_POINT ( 'NONE',  ( -11.73070664223723014, 231.3073905601784475, 11.32908994701042005 ) ) ;
#12090 = CARTESIAN_POINT ( 'NONE',  ( -13.20868407381884602, 248.2448905683720000, 6.410867750099229490 ) ) ;
#12091 = B_SPLINE_CURVE_WITH_KNOTS ( 'NONE', 1,
 ( #2338, #3844 ),
 .UNSPECIFIED., .F., .F.,
 ( 2, 2 ),
 ( 0.000000000000000000, 1.000000000000000000 ),
 .UNSPECIFIED. ) ;
#12092 = CARTESIAN_POINT ( 'NONE',  ( -45.43829269268871229, 365.3698905683720568, 0.000000000000000000 ) ) ;
#12093 = LINE ( 'NONE', #10353, #3717 ) ;
#12094 =( BOUNDED_CURVE ( )  B_SPLINE_CURVE ( 2, ( #16575, #15167, #1761, #13432, #19694, #8331, #14953, #140, #16683, #5302, #1871, #8441, #3581, #5199, #247, #20025, #11797 ),
 .UNSPECIFIED., .F., .T. ) 
 B_SPLINE_CURVE_WITH_KNOTS ( ( 3, 2, 2, 2, 2, 2, 2, 2, 3 ),
 ( 0.2968750000000001110, 0.2988281250000001110, 0.3007812500000001110, 0.3027343750000001110, 0.3046875000000001110, 0.3066406250000001110, 0.3085937500000001110, 0.3105468750000001110, 0.3125000000000001110 ),
 .UNSPECIFIED. ) 
 CURVE ( )  GEOMETRIC_REPRESENTATION_ITEM ( )  RATIONAL_B_SPLINE_CURVE ( ( 0.9999999999999988898, 0.9807852804032315408, 1.000000000000000000, 0.9807852804032304306, 1.000000000000000000, 0.9807852804032304306, 1.000000000000000000, 0.9807852804032304306, 1.000000000000000000, 0.9807852804032304306, 1.000000000000000000, 0.9807852804032304306, 1.000000000000000000, 0.9807852804032304306, 1.000000000000000000, 0.9807852804032293204, 1.000000000000001110 ) ) 
 REPRESENTATION_ITEM ( '' )  );
#12095 = CARTESIAN_POINT ( 'NONE',  ( -25.35362745456398414, 396.6823905683720000, 16.75240474999998952 ) ) ;
#12096 = CARTESIAN_POINT ( 'NONE',  ( 146.1533239063698772, 585.7448905601785327, -7.500000000000000000 ) ) ;
#12097 = CLOSED_SHELL ( 'NONE', ( #10200, #17932, #9558, #16893, #9929, #19732, #10052, #10488, #976, #10927, #13281, #17570, #15938, #9175, #4029, #9704 ) ) ;
#12098 = CARTESIAN_POINT ( 'NONE',  ( -14.54375231895777532, 403.4948905601784759, -14.14213562373094746 ) ) ;
#12099 = ORIENTED_EDGE ( 'NONE', *, *, #8908, .F. ) ;
#12100 = CARTESIAN_POINT ( 'NONE',  ( -28.68588794268874054, 588.2448905601785327, 0.000000000000000000 ) ) ;
#12101 = ORIENTED_EDGE ( 'NONE', *, *, #3929, .T. ) ;
#12102 = ORIENTED_EDGE ( 'NONE', *, *, #8908, .T. ) ;
#12103 = CARTESIAN_POINT ( 'NONE',  ( -13.20868407381887799, 519.7448905683720568, 6.410867750099229490 ) ) ;
#12104 = CARTESIAN_POINT ( 'NONE',  ( -28.68588794268870856, 294.7448905601784759, -19.99999999999999289 ) ) ;
#12105 = CARTESIAN_POINT ( 'NONE',  ( -32.66413529028186247, 319.8073905765655809, -19.99999999999999289 ) ) ;
#12106 = CARTESIAN_POINT ( 'NONE',  ( -11.93348319268871727, 330.3698905683720000, -2.051577885510841163E-15 ) ) ;
#12107 = CIRCLE ( 'NONE', #8302, 5.000000000000004441 ) ;
#12108 = EDGE_LOOP ( 'NONE', ( #897, #19848, #3983, #3679 ) ) ;
#12109 = CARTESIAN_POINT ( 'NONE',  ( -11.93348319268871904, 348.8698905683720568, -2.051577885510841163E-15 ) ) ;
#12110 = CARTESIAN_POINT ( 'NONE',  ( -45.43829269268871229, 373.8698905683720000, 0.000000000000000000 ) ) ;
#12111 = AXIS2_PLACEMENT_3D ( 'NONE', #4610, #11407, #18012 ) ;
#12112 = CARTESIAN_POINT ( 'NONE',  ( -28.68588794268870856, 289.4948905765656377, -19.99999999999999289 ) ) ;
#12113 = VECTOR ( 'NONE', #15912, 1000.000000000000000 ) ;
#12114 = CARTESIAN_POINT ( 'NONE',  ( 51.98438129372387806, -133.1434774248255906, -117.7249735956185219 ) ) ;
#12115 = CARTESIAN_POINT ( 'NONE',  ( -16.84014894278197616, 267.6198905683720568, 11.84573899990672530 ) ) ;
#12116 = CARTESIAN_POINT ( 'NONE',  ( -43.68588794268869435, 200.1437886375728965, -2.037320803886357560E-15 ) ) ;
#12117 = AXIS2_PLACEMENT_3D ( 'NONE', #19609, #19190, #9333 ) ;
#12118 = EDGE_CURVE ( 'NONE', #21094, #19703, #1451, .T. ) ;
#12119 = CARTESIAN_POINT ( 'NONE',  ( -22.27502019258949417, 412.2448905683720568, -15.47720386886985544 ) ) ;
#12120 = LINE ( 'NONE', #2075, #4745 ) ;
#12121 = CARTESIAN_POINT ( 'NONE',  ( -14.54375231895776821, 353.4948905601785327, -14.14213562373094746 ) ) ;
#12122 = AXIS2_PLACEMENT_3D ( 'NONE', #18890, #15773, #962 ) ;
#12123 = CARTESIAN_POINT ( 'NONE',  ( -47.16347859291445133, 407.8698905601784759, 7.653668647301805628 ) ) ;
#12124 = CARTESIAN_POINT ( 'NONE',  ( -35.09675569278794427, 333.4948905683720568, -15.47720386886985544 ) ) ;
#12125 = CARTESIAN_POINT ( 'NONE',  ( -28.68588794268872988, 471.3698905683720568, -16.75240474999999307 ) ) ;
#12126 = ORIENTED_EDGE ( 'NONE', *, *, #18225, .F. ) ;
#12127 = CARTESIAN_POINT ( 'NONE',  ( -17.35679799567830273, 460.6823905601784759, 16.95518130045146421 ) ) ;
#12128 = CARTESIAN_POINT ( 'NONE',  ( -13.20868407381884957, 288.2448905683720000, 6.410867750099229490 ) ) ;
#12129 = ADVANCED_FACE ( 'NONE', ( #6088 ), #19293, .T. ) ;
#12130 = ORIENTED_EDGE ( 'NONE', *, *, #18674, .T. ) ;
#12131 = CARTESIAN_POINT ( 'NONE',  ( -24.70764059509554755, 340.0573905601784190, 19.99999999999998934 ) ) ;
#12132 = ORIENTED_EDGE ( 'NONE', *, *, #18687, .T. ) ;
#12133 = FACE_OUTER_BOUND ( 'NONE', #18801, .T. ) ;
#12134 = CARTESIAN_POINT ( 'NONE',  ( -42.82802356641965957, 338.4948905601785327, 14.14213562373094923 ) ) ;
#12135 = EDGE_CURVE ( 'NONE', #6677, #11766, #12478, .T. ) ;
#12136 = CARTESIAN_POINT ( 'NONE',  ( -40.53162694259543031, 292.6198905683720000, -11.84573899990672707 ) ) ;
#12137 = ADVANCED_FACE ( 'NONE', ( #8350 ), #6941, .F. ) ;
#12138 = CARTESIAN_POINT ( 'NONE',  ( -38.17536295476244845, 386.9323905683721136, 14.20200298773971781 ) ) ;
#12139 = CARTESIAN_POINT ( 'NONE',  ( -17.35679799567829562, 373.8073905601784759, -16.95518130045146421 ) ) ;
#12140 = CARTESIAN_POINT ( 'NONE',  ( -8.685887942688744090, 526.6823905765655809, 3.978247347593161010 ) ) ;
#12141 = CARTESIAN_POINT ( 'NONE',  ( -19.19641293061498999, 410.4323905683720568, -14.20200298773971603 ) ) ;
#12142 = CARTESIAN_POINT ( 'NONE',  ( -40.53162694259542320, 254.1198905683720284, -11.84573899990672707 ) ) ;
#12143 = CARTESIAN_POINT ( 'NONE',  ( -45.43829269268871940, 423.5573905683720000, -3.332260488124726638 ) ) ;
#12144 = ITEM_DEFINED_TRANSFORMATION ( 'NONE', 'NONE', #4845,  #12794 ) ;
#12145 = CARTESIAN_POINT ( 'NONE',  ( -28.68588794268871212, 344.4948905765656377, 19.99999999999999289 ) ) ;
#12146 = CARTESIAN_POINT ( 'NONE',  ( -8.685887942688708563, 236.9948905765656377, -2.449293598294705724E-15 ) ) ;
#12147 = CARTESIAN_POINT ( 'NONE',  ( -13.20868407381885490, 328.2448905683720000, 6.410867750099229490 ) ) ;
#12148 = CARTESIAN_POINT ( 'NONE',  ( -40.53162694259545162, 484.1198905683720000, -11.84573899990672707 ) ) ;
#12149 = ADVANCED_FACE ( 'NONE', ( #3288 ), #16911, .T. ) ;
#12150 = CARTESIAN_POINT ( 'NONE',  ( 125.7989814974898053, 10.52886280891152104, 40.00000000000000000 ) ) ;
#12151 = CARTESIAN_POINT ( 'NONE',  ( -43.47668584505344569, 200.8081422174835211, -2.511554223531087260 ) ) ;
#12152 = MECHANICAL_DESIGN_GEOMETRIC_PRESENTATION_REPRESENTATION (  '', ( #14239 ), #15962 ) ;
#12153 = CARTESIAN_POINT ( 'NONE',  ( -8.685887942688795604, 226.6823905765656377, 3.978247347593374172 ) ) ;
#12154 = CARTESIAN_POINT ( 'NONE',  ( -19.19641293061498644, 378.8073905683721136, 14.20200298773971426 ) ) ;
#12155 = CARTESIAN_POINT ( 'NONE',  ( -27.39255831251362139, 46.46955322709327163, -121.9637379996554216 ) ) ;
#12156 = CARTESIAN_POINT ( 'NONE',  ( -17.35679799567831694, 523.8073905601785327, -16.95518130045146421 ) ) ;
#12157 = CARTESIAN_POINT ( 'NONE',  ( -22.27502019258948707, 350.7448905683720568, -15.47720386886985544 ) ) ;
#12158 = EDGE_LOOP ( 'NONE', ( #6248, #12021, #3854, #2401, #16936, #1521 ) ) ;
#12159 = CARTESIAN_POINT ( 'NONE',  ( -22.27502019258949417, 506.9948905683721136, 15.47720386886985189 ) ) ;
#12160 = ORIENTED_EDGE ( 'NONE', *, *, #10215, .F. ) ;
#12161 = MANIFOLD_SOLID_BREP ( 'Fillet4', #1762 ) ;
#12162 = CARTESIAN_POINT ( 'NONE',  ( -28.68588794268871212, 349.7448905601784759, 19.99999999999999289 ) ) ;
#12163 = CARTESIAN_POINT ( 'NONE',  ( -36.33955658999050797, 380.1198905765656377, -18.47759065022572855 ) ) ;
#12164 = CARTESIAN_POINT ( 'NONE',  ( -10.76731745429009912, 50.09631838541057647, 118.3724535612433186 ) ) ;
#12165 = DIRECTION ( 'NONE',  ( 9.855701800883827197E-17, -1.000000000000000000, 0.000000000000000000 ) ) ;
#12166 = CARTESIAN_POINT ( 'NONE',  ( -32.01814843081346140, 466.0573905683720000, 16.75240474999999307 ) ) ;
#12167 = AXIS2_PLACEMENT_3D ( 'NONE', #4306, #15568, #4194 ) ;
#12168 = VERTEX_POINT ( 'NONE', #14870 ) ;
#12169 = CARTESIAN_POINT ( 'NONE',  ( -25.35362745456400546, 481.0573905683720568, -16.75240474999999307 ) ) ;
#12170 =( BOUNDED_CURVE ( )  B_SPLINE_CURVE ( 2, ( #8024, #14230, #1240, #20818, #12701, #4478, #14656, #7814, #15954, #6403, #10955, #5988, #12598, #11061, #14444, #6194, #19398 ),
 .UNSPECIFIED., .F., .T. ) 
 B_SPLINE_CURVE_WITH_KNOTS ( ( 3, 2, 2, 2, 2, 2, 2, 2, 3 ),
 ( 0.4218750000000001665, 0.4238281250000001665, 0.4257812500000001665, 0.4277343750000001665, 0.4296875000000002220, 0.4316406250000002220, 0.4335937500000002220, 0.4355468750000002220, 0.4375000000000002220 ),
 .UNSPECIFIED. ) 
 CURVE ( )  GEOMETRIC_REPRESENTATION_ITEM ( )  RATIONAL_B_SPLINE_CURVE ( ( 0.9999999999999983347, 0.9807852804032320959, 1.000000000000000000, 0.9807852804032304306, 1.000000000000000000, 0.9807852804032304306, 1.000000000000000000, 0.9807852804032304306, 1.000000000000000000, 0.9807852804032304306, 1.000000000000000000, 0.9807852804032304306, 1.000000000000000000, 0.9807852804032304306, 1.000000000000000000, 0.9807852804032282101, 1.000000000000002220 ) ) 
 REPRESENTATION_ITEM ( '' )  );
#12171 = LINE ( 'NONE', #1040, #12417 ) ;
#12172 = CARTESIAN_POINT ( 'NONE',  ( -24.70764059509556887, 419.1823905765655809, -19.99999999999999289 ) ) ;
#12173 = CARTESIAN_POINT ( 'NONE',  ( -14.54375231895778064, 475.7448905765655809, 14.14213562373094568 ) ) ;
#12174 = DIRECTION ( 'NONE',  ( -0.000000000000000000, -0.000000000000000000, -1.000000000000000000 ) ) ;
#12175 = CARTESIAN_POINT ( 'NONE',  ( -42.82802356641967378, 485.9948905601784759, -14.14213562373094746 ) ) ;
#12176 = LINE ( 'NONE', #4277, #19769 ) ;
#12177 = CARTESIAN_POINT ( 'NONE',  ( -1.025382690249029949, 303.6587712403113528, 25.00000000000000000 ) ) ;
#12178 = FILL_AREA_STYLE_COLOUR ( '', #14257 ) ;
#12179 = DIRECTION ( 'NONE',  ( 0.000000000000000000, 0.9253149302858357794, -0.3791995250394160633 ) ) ;
#12180 = AXIS2_PLACEMENT_3D ( 'NONE', #16523, #2030, #90 ) ;
#12181 = CARTESIAN_POINT ( 'NONE',  ( -32.01814843081344009, 283.1823905683720568, -16.75240474999999307 ) ) ;
#12182 = CARTESIAN_POINT ( 'NONE',  ( -47.16347859291443001, 247.8698905601785043, 7.653668647301805628 ) ) ;
#12183 = CARTESIAN_POINT ( 'NONE',  ( 60.03793209889851568, 30.52886280891152282, -152.3753892284480003 ) ) ;
#12184 = CARTESIAN_POINT ( 'NONE',  ( -45.43829269268871940, 455.6823905683720000, 3.332260488124734632 ) ) ;
#12185 = DIRECTION ( 'NONE',  ( 0.000000000000000000, -0.000000000000000000, -1.000000000000000000 ) ) ;
#12186 = CARTESIAN_POINT ( 'NONE',  ( -38.17536295476244135, 263.8073905683720568, -14.20200298773971426 ) ) ;
#12187 = ORIENTED_EDGE ( 'NONE', *, *, #7343, .T. ) ;
#12188 = CARTESIAN_POINT ( 'NONE',  ( -47.16347859291445843, 481.3698905765655809, -7.653668647301793193 ) ) ;
#12189 = CARTESIAN_POINT ( 'NONE',  ( -19.19641293061500065, 491.9323905683720000, -14.20200298773971603 ) ) ;
#12190 = ADVANCED_FACE ( 'NONE', ( #11713 ), #6620, .F. ) ;
#12191 = VERTEX_POINT ( 'NONE', #13241 ) ;
#12192 = CYLINDRICAL_SURFACE ( 'NONE', #724, 19.99999999999999645 ) ;
#12193 = CARTESIAN_POINT ( 'NONE',  ( -28.68588794268869790, 236.3698905683720568, 16.75240474999999307 ) ) ;
#12194 = VERTEX_POINT ( 'NONE', #11818 ) ;
#12195 = DIRECTION ( 'NONE',  ( 0.000000000000000000, 0.000000000000000000, 1.000000000000000000 ) ) ;
#12196 = CARTESIAN_POINT ( 'NONE',  ( -40.01497788969914637, 473.5573905765655809, 16.95518130045146776 ) ) ;
#12197 = CARTESIAN_POINT ( 'NONE',  ( 0.000000000000000000, 5.629165124598848102, 3.250000000000005329 ) ) ;
#12198 = PRODUCT_RELATED_PRODUCT_CATEGORY ( 'part', '', ( #5946 ) ) ;
#12199 = DIRECTION ( 'NONE',  ( 1.000000000000000000, 0.000000000000000000, 0.000000000000000000 ) ) ;
#12200 = CARTESIAN_POINT ( 'NONE',  ( -32.01814843081343298, 247.5573905683720000, 16.75240474999999307 ) ) ;
#12201 = CARTESIAN_POINT ( 'NONE',  ( -44.16309181155858710, 515.9948905683720568, 6.410867750099241924 ) ) ;
#12202 = DIRECTION ( 'NONE',  ( 0.000000000000000000, -1.000000000000000000, 0.000000000000000000 ) ) ;
#12203 = CARTESIAN_POINT ( 'NONE',  ( -25.35362745456396638, 246.6823905683720284, 16.75240474999998952 ) ) ;
#12204 = CARTESIAN_POINT ( 'NONE',  ( -45.43829269268871229, 335.3698905683720000, 0.000000000000000000 ) ) ;
#12205 = EDGE_CURVE ( 'NONE', #502, #8850, #1561, .T. ) ;
#12206 = AXIS2_PLACEMENT_3D ( 'NONE', #12100, #10792, #15262 ) ;
#12207 = DIRECTION ( 'NONE',  ( -1.000000000000000000, 0.000000000000000000, 0.000000000000000000 ) ) ;
#12208 = VECTOR ( 'NONE', #19409, 1000.000000000000000 ) ;
#12209 = CARTESIAN_POINT ( 'NONE',  ( -38.17536295476246266, 402.3073905683720000, -14.20200298773971426 ) ) ;
#12210 = UNCERTAINTY_MEASURE_WITH_UNIT (LENGTH_MEASURE( 1.000000000000000082E-05 ), #16096, 'distance_accuracy_value', 'NONE');
#12211 = CARTESIAN_POINT ( 'NONE',  ( -28.68588794268870856, 324.4948905765655809, 19.99999999999999289 ) ) ;
#12212 = CARTESIAN_POINT ( 'NONE',  ( -28.68588794268871567, 399.7448905601784759, 19.99999999999999289 ) ) ;
#12213 = EDGE_CURVE ( 'NONE', #20916, #10281, #6835, .T. ) ;
#12214 = ORIENTED_EDGE ( 'NONE', *, *, #18138, .F. ) ;
#12215 = ADVANCED_FACE ( 'NONE', ( #18412 ), #16806, .T. ) ;
#12216 = CARTESIAN_POINT ( 'NONE',  ( -48.68588794268861619, 351.6823905765656946, -3.978247347593371508 ) ) ;
#12217 = VERTEX_POINT ( 'NONE', #18619 ) ;
#12218 = ORIENTED_EDGE ( 'NONE', *, *, #6962, .F. ) ;
#12219 = CARTESIAN_POINT ( 'NONE',  ( -25.35362745456400901, 512.5573905683719431, -16.75240474999999307 ) ) ;
#12220 = CARTESIAN_POINT ( 'NONE',  ( -14.54375231895776466, 318.2448905765656377, -14.14213562373094746 ) ) ;
#12221 = VERTEX_POINT ( 'NONE', #4242 ) ;
#12222 = AXIS2_PLACEMENT_3D ( 'NONE', #16854, #15025, #13711 ) ;
#12223 = CARTESIAN_POINT ( 'NONE',  ( -42.88789093042842637, 304.4323905683720000, -9.489475012073734561 ) ) ;
#12224 = ORIENTED_EDGE ( 'NONE', *, *, #13921, .F. ) ;
#12225 = CARTESIAN_POINT ( 'NONE',  ( -32.01814843081344719, 346.0573905683720568, 16.75240474999999307 ) ) ;
#12226 = CARTESIAN_POINT ( 'NONE',  ( -38.17536295476245556, 352.3073905683719431, -14.20200298773971426 ) ) ;
#12227 = VECTOR ( 'NONE', #13203, 1000.000000000000000 ) ;
#12228 = CARTESIAN_POINT ( 'NONE',  ( -21.03221929538690205, 285.1198905765656377, 18.47759065022572500 ) ) ;
#12229 = CARTESIAN_POINT ( 'NONE',  ( -45.64106924314019409, 501.0573905765656377, -11.32908994701042538 ) ) ;
#12230 = CARTESIAN_POINT ( 'NONE',  ( -40.53162694259542320, 245.1198905683720284, 11.84573899990672885 ) ) ;
#12231 = PLANE ( 'NONE',  #496 ) ;
#12232 =( BOUNDED_CURVE ( )  B_SPLINE_CURVE ( 2, ( #4507, #6122, #19219, #9579, #15989, #12730, #9477, #10772, #19000, #21160, #6334, #16088, #14371, #17805, #21054, #14473, #1170, #4186, #1267, #6224, #11097, #19321, #17486, #7844, #7742, #16195, #7944, #17700, #11207, #4297, #12839, #17388, #1374, #10881, #14576, #2995, #2571, #9150, #15879, #14151, #15772, #7526, #20738, #2786, #12628, #2676, #5911, #19115, #6019, #9262, #1068, #7637, #4402, #9373, #14262, #20849, #10985, #17594, #4816, #11744, #3099, #14789, #19636, #21264, #18336, #13158, #12946, #18120, #15112, #16306, #16517, #15006, #11410, #8056, #4930, #14687, #8382, #3422, #1479, #10113, #13047, #3315, #9894, #3208, #5034, #18230, #16734, #1921, #11308, #8489, #296, #9787, #9682, #13377, #6432, #19534, #18015, #16624, #16410, #1588, #8158, #21373, #6541, #19746, #17904, #11527, #1699, #5146, #8267, #14898, #84, #4711, #6650, #13272, #19857, #10001, #11635, #1815, #192, #6759, #19967, #2332, #10426, #13484, #18756, #8913, #20389, #510, #15215, #17047, #18445, #406, #15643, #5250, #6865, #7176, #3731, #15426, #6971, #5455, #11849, #10529, #20077, #8809, #10316, #2024, #3631, #10213, #8703, #18544, #16836, #12278, #611, #13693, #7073, #5563, #13798, #16940, #11950, #13594, #20181, #2122, #5349, #15325, #20285, #5670, #8592, #12057, #17151, #12169, #18645, #3837, #3944, #7287, #2228, #15534, #20500, #715, #13911, #18859, #4049, #10638, #17256, #2439, #9020, #2972, #9125, #12602, #19194, #12496, #14344, #6091, #21028, #12811, #20600, #6198, #11177, #19087, #12380, #1243, #15747, #19402, #9337, #9550, #17779, #18973, #4482, #14123, #17460, #17361, #5773, #934, #7500, #14448, #10856, #20710, #15855, #14021, #828, #10959, #4373, #17568, #7394, #2760, #4269, #15958, #17672, #4154, #7817, #10746, #20924, #7715, #1144, #1039, #4585, #12705, #19297, #11065, #2542, #5883, #2649, #9235, #2866, #7603, #9449, #14234, #20823, #5992, #16067, #12918, #16170, #17878, #21133, #14548, #5008, #13019, #3396, #6306, #52, #19507, #1346, #14977, #18199, #11608, #19718, #7919, #6622, #9976, #8241, #9761, #3071, #4902, #4685, #9655, #3497, #11280, #16277, #16490, #19611, #3290, #1453, #8026, #19938, #19833, #14659, #18095, #4788, #21240, #6406, #11385, #17984, #3182, #16385, #164, #9864, #1560, #8130, #14872, #1672, #14762, #21347, #6515, #13131, #11498, #13243, #16596, #1786, #6735, #8353, #13350, #5116, #11716, #18308, #10084, #15402, #10507, #3604, #18622, #2307, #13670, #13568, #5223, #2096, #11821, #5538, #585, #20046, #15507, #10188, #15299, #18415, #5646, #16809, #12253, #12030, #2201, #20363, #20476, #1894, #7153, #13885, #17128, #1999, #692, #8568, #13774, #271, #20156, #6945, #16706, #15189, #18836, #3810, #12143, #8890, #18731, #8461, #6838, #374, #5324, #15086, #20259, #5430, #3917, #11925, #18519, #3705, #8675, #10293, #7261, #13454, #16914, #486, #7050, #10401, #17020, #8786, #13997, #6174, #5965, #17544, #2415, #2842, #14425, #15723, #15616, #4454, #12357, #16044, #4129, #7692, #804, #7472, #908, #10614, #20578, #7792, #12578, #9314, #11039, #6068, #14102, #18944, #19063, #17232, #21006, #14209, #7581, #15932, #5746, #17335, #2519, #15831, #8995, #4350, #10718, #20683, #9102, #5858, #7369, #4021, #1222, #1015, #19172, #1120, #12466, #4246, #12785, #10830, #14321, #20797, #9425, #12679, #20900, #10933, #17440, #19273, #17650, #2734, #2624, #9206, #1645, #16357, #16569, #8327, #8105, #11582, #4664, #3263, #17755, #1755, #11255, #14949, #8217, #11151, #21317, #16250, #14523, #2946, #9525, #21218, #3157, #12992, #17854, #1535, #21, #6383, #6597, #18068, #13218, #19585, #9736, #14735, #9631, #19484, #12895, #3048, #18173, #16143, #1324, #14846, #6488, #19378, #9839, #19805, #1429, #13105, #3371, #19690, #8001, #9949, #4876, #21109, #11470, #7895, #4983, #16462, #4765, #14634, #136, #6709, #4563, #6280, #11360, #17957, #6812, #13428, #8644, #3577, #5510, #2279, #16995, #12110, #1970, #15163, #20019, #242, #18703, #13540, #13326, #18492, #456, #3889, #16885, #16784, #10478, #2069, #8541, #7125, #15272, #2173, #20230, #15480, #5195, #3681, #10266, #10166, #5400, #18596, #17100, #8859, #665, #5089, #3780, #19908, #12005, #11690, #20129, #18281, #7022, #3469, #10056, #16679, #8759, #11792, #351, #8437, #1867, #18388, #6914, #15060, #5297, #11899, #13644, #10370, #15378, #556, #13751, #20337, #13855, #17417, #4101, #9179, #2709, #5618, #14581, #10582, #5939, #14180, #15804, #7446, #12226, #18809, #17518, #10689, #16200, #3991, #12553, #17205, #20445, #10907, #16311, #1378, #7231, #12950, #19147, #20554, #13971, #17908, #991, #5720, #2384, #15591, #8967, #776, #7338, #7555, #17308, #20771, #12328, #5827, #18916, #10802, #15695, #2599, #20657, #14072, #19034, #4220, #2493, #4324, #9585, #7950, #21165, #3105, #9075, #6337, #11314, #19539, #882, #12437, #4716, #9688, #13889, #15512, #16711, #8790, #18422, #381, #277, #10090, #5541, #7157, #5122, #1900, #10194, #8573, #8468, #11722, #13779, #11828, #8679, #18314, #15303, #2005, #7055, #589, #3504, #12147, #15092, #3814, #6845, #13460, #20053, #5229, #3609, #15409, #15196, #20367, #16816, #10406, #6951, #13572, #18736, #20162, #3920, #5329, #10510, #17023, #11930, #18523, #3709, #10296, #490, #16920, #2101, #13673, #20263, #5433, #12034, #18626, #2204, #17132, #2312, #8894, #695, #7265, #2628, #12470, #20688, #15619, #18839, #913, #10722, #4026, #4457, #1020, #5863, #19066, #19175, #20800, #17338, #4132, #14001, #20581, #15833, #2523, #12683, #9429, #2738, #19276, #10619, #9318, #12581, #10835, #20479, #4353, #20903, #5751, #7584, #11042, #9212, #9105, #17653, #14213, #15726, #14324, #5968, #15935, #10937, #1225, #5650, #17548, #7475, #1124, #7695, #17235, #6071, #2418, #2845, #16047, #7796, #4249, #12256, #17442, #8999, #807, #7373, #12361, #18951, #14105, #21009, #18071, #1760, #8221, #14429, #19809, #13109, #6283, #21112, #3375, #8109, #12898, #3267, #11364, #11585, #9952, #3161, #6600, #19487, #19693, #18177, #4668, #16574, #9842, #6178, #16360, #11258, #9528, #12788, #19381, #16253, #17858, #4566, #4986, #1538, #21222, #14637, #4879, #14740, #3051, #8004, #4769, #17960, #9635, #14526, #7898, #1432, #13221, #11155, #17759, #16466, #6492, #9739, #2949, #11474, #14850, #6386, #21322, #16147, #1649, #12997, #1327, #19590, #24, #3784, #20233, #18285, #13754, #8440, #13543, #16682, #3892, #3474, #10483, #10271, #459, #18601, #18706, #139, #13648, #19912, #8762, #1870, #20340, #15064, #12009, #5093, #11796, #5198, #14952, #10060, #12115, #16888, #5404, #15382, #10375, #8330, #11694, #13431, #18392, #17103, #18495, #11902, #16998, #246, #2177, #3684, #561, #15276, #6713, #6816, #20133, #5301, #20024, #7026, #7128, #5515, #13329, #3580, #10169, #16787, #1975, #8545, #15166, #355, #6919, #2072, #8649, #12655, #13861, #5942, #15595, #18920, #18813, #7234, #17208, #2387, #15908, #12332, #8970, #5724, #20448, #2283, #4327, #780, #5831, #8863, #12440, #20557, #4223, #19152, #668, #9293, #5621, #995, #9182, #10806, #2496, #14296, #20660, #12557, #4104, #10910, #12230, #7558, #3994, #15483, #17522, #11016, #2712, #10587, #7669, #14184, #7341, #13975, #19250, #17421, #10692, #1100, #19039, #17313, #9078, #15699, #2602, #885, #15808, #7449, #14077, #20776, #20881, #6047, #4432, #9610, #17832, #12762, #3131, #20982, #3241, #1405, #11235, #19562, #3028, #16228, #16337, #17935, #7873, #1299, #11126, #17731, #12972, #14502, #9816, #6573, #21292, #16440, #6258, #19460, #2925, #4541, #1619, #1511, #18047, #9505, #4743, #8192, #21193, #21085, #14821, #6362, #12870, #11341, #4644 ),
 .UNSPECIFIED., .F., .T. ) 
 B_SPLINE_CURVE_WITH_KNOTS ( ( 3, 2, 2, 2, 2, 2, 2, 2, 2, 2, 2, 2, 2, 2, 2, 2, 2, 2, 2, 2, 2, 2, 2, 2, 2, 2, 2, 2, 2, 2, 2, 2, 2, 2, 2, 2, 2, 2, 2, 2, 2, 2, 2, 2, 2, 2, 2, 2, 2, 2, 2, 2, 2, 2, 2, 2, 2, 2, 2, 2, 2, 2, 2, 2, 2, 2, 2, 2, 2, 2, 2, 2, 2, 2, 2, 2, 2, 2, 2, 2, 2, 2, 2, 2, 2, 2, 2, 2, 2, 2, 2, 2, 2, 2, 2, 2, 2, 2, 2, 2, 2, 2, 2, 2, 2, 2, 2, 2, 2, 2, 2, 2, 2, 2, 2, 2, 2, 2, 2, 2, 2, 2, 2, 2, 2, 2, 2, 2, 2, 2, 2, 2, 2, 2, 2, 2, 2, 2, 2, 2, 2, 2, 2, 2, 2, 2, 2, 2, 2, 2, 2, 2, 2, 2, 2, 2, 2, 2, 2, 2, 2, 2, 2, 2, 2, 2, 2, 2, 2, 2, 2, 2, 2, 2, 2, 2, 2, 2, 2, 2, 2, 2, 2, 2, 2, 2, 2, 2, 2, 2, 2, 2, 2, 2, 2, 2, 2, 2, 2, 2, 2, 2, 2, 2, 2, 2, 2, 2, 2, 2, 2, 2, 2, 2, 2, 2, 2, 2, 2, 2, 2, 2, 2, 2, 2, 2, 2, 2, 2, 2, 2, 2, 2, 2, 2, 2, 2, 2, 2, 2, 2, 2, 2, 2, 2, 2, 2, 2, 2, 2, 2, 2, 2, 2, 2, 2, 2, 2, 2, 2, 2, 2, 2, 2, 2, 2, 2, 2, 2, 2, 2, 2, 2, 2, 2, 2, 2, 2, 2, 2, 2, 2, 2, 2, 2, 2, 2, 2, 2, 2, 2, 2, 2, 2, 2, 2, 2, 2, 2, 2, 2, 2, 2, 2, 2, 2, 2, 2, 2, 2, 2, 2, 2, 2, 2, 2, 2, 2, 2, 2, 2, 2, 2, 2, 2, 2, 2, 2, 2, 2, 2, 2, 2, 2, 2, 2, 2, 2, 2, 2, 2, 2, 2, 2, 2, 2, 2, 2, 2, 2, 2, 2, 2, 2, 2, 2, 2, 2, 2, 2, 2, 2, 2, 2, 2, 2, 2, 2, 2, 2, 2, 2, 2, 2, 2, 2, 2, 2, 2, 2, 2, 2, 2, 2, 2, 2, 2, 2, 2, 2, 2, 2, 2, 2, 2, 2, 2, 2, 2, 2, 2, 2, 2, 2, 2, 2, 2, 2, 2, 2, 2, 2, 2, 2, 2, 2, 2, 2, 2, 2, 2, 2, 2, 2, 2, 2, 2, 2, 2, 2, 2, 2, 2, 2, 2, 2, 2, 2, 2, 2, 2, 2, 2, 2, 2, 2, 2, 2, 2, 2, 2, 2, 2, 2, 2, 2, 2, 2, 2, 2, 2, 2, 2, 2, 2, 2, 2, 2, 2, 2, 2, 2, 2, 2, 2, 2, 2, 2, 2, 2, 2, 2, 2, 2, 2, 2, 2, 2, 2, 2, 2, 2, 2, 2, 2, 2, 3 ),
 ( 0.000000000000000000, 0.001994670335415893447, 0.003989340670831786895, 0.005984011006247681209, 0.007978681341663573789, 0.009973351677079468972, 0.01196802201249536242, 0.01396269234791125587, 0.01595736268332714758, 0.01795203301874304103, 0.01994670335415893794, 0.02194137368957482792, 0.02393604402499072484, 0.02593071436040661482, 0.02792538469582251173, 0.02992005503123840171, 0.03191472536665429516, 0.03390939570207018861, 0.03590406603748608205, 0.03789873637290198244, 0.03989340670831787589, 0.04188807704373376239, 0.04388274737914965584, 0.04587741771456555623, 0.04787208804998144968, 0.04986675838539734312, 0.05186142872081322963, 0.05385609905622912308, 0.05585076939164502347, 0.05784543972706091691, 0.05984011006247680342, 0.06183478039789269687, 0.06382945073330859032, 0.06582412106872448376, 0.06781879140414037721, 0.06981346173955627066, 0.07180813207497216411, 0.07380280241038805755, 0.07579747274580396488, 0.07779214308121985832, 0.07978681341663575177, 0.08178148375205164522, 0.08377615408746752479, 0.08577082442288341824, 0.08776549475829931168, 0.08976016509371520513, 0.09175483542913111246, 0.09374950576454700590, 0.09574417609996289935, 0.09773884643537879280, 0.09973351677079468625, 0.1017281871062105658, 0.1037228574416264593, 0.1057175277770423527, 0.1077121981124582462, 0.1097068684478741535, 0.1117015387832900469, 0.1136962091187059404, 0.1156908794541218338, 0.1176855497895377273, 0.1196802201249536068, 0.1216748904603695003, 0.1236695607957853937, 0.1256642311312012872, 0.1276589014666171806, 0.1296535718020330741, 0.1316482421374489675, 0.1336429124728648887, 0.1356375828082807544, 0.1376322531436966756, 0.1396269234791125413, 0.1416215938145284625, 0.1436162641499443282, 0.1456109344853602494, 0.1476056048207761151, 0.1496002751561920086, 0.1515949454916079298, 0.1535896158270237954, 0.1555842861624397166, 0.1575789564978555823, 0.1595736268332715035, 0.1615682971686873692, 0.1635629675041032904, 0.1655576378395191561, 0.1675523081749350496, 0.1695469785103509708, 0.1715416488457668365, 0.1735363191811827577, 0.1755309895165986234, 0.1775256598520145446, 0.1795203301874304103, 0.1815150005228463315, 0.1835096708582622249, 0.1855043411936780906, 0.1874990115290940118, 0.1894936818645098775, 0.1914883521999257987, 0.1934830225353416644, 0.1954776928707575856, 0.1974723632061734513, 0.1994670335415893725, 0.2014617038770052659, 0.2034563742124211316, 0.2054510445478370528, 0.2074457148832529185, 0.2094403852186688397, 0.2114350555540847054, 0.2134297258895006266, 0.2154243962249164923, 0.2174190665603324135, 0.2194137368957483070, 0.2214084072311641727, 0.2234030775665800939, 0.2253977479019959596, 0.2273924182374118808, 0.2293870885728277464, 0.2313817589082436676, 0.2333764292436595611, 0.2353710995790754545, 0.2373657699144913480, 0.2393604402499072137, 0.2413551105853231349, 0.2433497809207390006, 0.2453444512561549218, 0.2473391215915707875, 0.2493337919269867087, 0.2513284622624025744, 0.2533231325978185233, 0.2553178029332343613, 0.2573124732686502547, 0.2593071436040661482, 0.2613018139394820971, 0.2632964842748979351, 0.2652911546103138285, 0.2672858249457297775, 0.2692804952811456709, 0.2712751656165615088, 0.2732698359519774023, 0.2752645062873933512, 0.2772591766228091892, 0.2792538469582250826, 0.2812485172936409761, 0.2832431876290569250, 0.2852378579644727630, 0.2872325282998886564, 0.2892271986353046054, 0.2912218689707204988, 0.2932165393061363368, 0.2952112096415522302, 0.2972058799769681792, 0.2992005503123840171, 0.3011952206477999106, 0.3031898909832158595, 0.3051845613186317530, 0.3071792316540475909, 0.3091739019894634843, 0.3111685723248794333, 0.3131632426602952712, 0.3151579129957111647, 0.3171525833311271136, 0.3191472536665430071, 0.3211419240019588450, 0.3231365943373747385, 0.3251312646727906874, 0.3271259350082065809, 0.3291206053436224188, 0.3311152756790383123, 0.3331099460144542612, 0.3351046163498700992, 0.3370992866852859926, 0.3390939570207019416, 0.3410886273561178350, 0.3430832976915336729, 0.3450779680269495664, 0.3470726383623655154, 0.3490673086977813533, 0.3510619790331972467, 0.3530566493686131957, 0.3550513197040290891, 0.3570459900394449271, 0.3590406603748608205, 0.3610353307102767695, 0.3630300010456926629, 0.3650246713811085009, 0.3670193417165244498, 0.3690140120519403433, 0.3710086823873561812, 0.3730033527227720747, 0.3749980230581880236, 0.3769926933936039171, 0.3789873637290197550, 0.3809820340644356484, 0.3829767043998515974, 0.3849713747352674353, 0.3869660450706833288, 0.3889607154060992777, 0.3909553857415151712, 0.3929500560769310091, 0.3949447264123469026, 0.3969393967477628515, 0.3989340670831787450, 0.4009287374185945829, 0.4029234077540105319, 0.4049180780894264253, 0.4069127484248422633, 0.4089074187602581567, 0.4109020890956741057, 0.4128967594310899991, 0.4148914297665058371, 0.4168861001019217860, 0.4188807704373376795, 0.4208754407727535174, 0.4228701111081694108, 0.4248647814435853598, 0.4268594517790012532, 0.4288541221144170912, 0.4308487924498329846, 0.4328434627852489336, 0.4348381331206648270, 0.4368328034560806650, 0.4388274737914966139, 0.4408221441269125074, 0.4428168144623283453, 0.4448114847977442388, 0.4468061551331601877, 0.4488008254685760812, 0.4507954958039919191, 0.4527901661394078681, 0.4547848364748237615, 0.4567795068102395994, 0.4587741771456554929, 0.4607688474810714419, 0.4627635178164873353, 0.4647581881519031732, 0.4667528584873191222, 0.4687475288227350156, 0.4707421991581509091, 0.4727368694935667470, 0.4747315398289826960, 0.4767262101643985894, 0.4787208804998144274, 0.4807155508352303208, 0.4827102211706462698, 0.4847048915060621632, 0.4866995618414780012, 0.4886942321768939501, 0.4906889025123098436, 0.4926835728477256815, 0.4946782431831415749, 0.4966729135185575239, 0.4986675838539734174, 0.5006622541893892553, 0.5026569245248051487, 0.5046515948602210422, 0.5066462651956370467, 0.5086409355310528291, 0.5106356058664687225, 0.5126302762018846160, 0.5146249465373005094, 0.5166196168727164029, 0.5186142872081322963, 0.5206089575435483008, 0.5226036278789641942, 0.5245982982143800877, 0.5265929685497958701, 0.5285876388852117636, 0.5305823092206276570, 0.5325769795560435504, 0.5345716498914595549, 0.5365663202268754484, 0.5385609905622913418, 0.5405556608977071242, 0.5425503312331230177, 0.5445450015685389111, 0.5465396719039548046, 0.5485343422393708090, 0.5505290125747867025, 0.5525236829102025959, 0.5545183532456183784, 0.5565130235810342718, 0.5585076939164501653, 0.5605023642518660587, 0.5624970345872819522, 0.5644917049226979566, 0.5664863752581138501, 0.5684810455935296325, 0.5704757159289455259, 0.5724703862643614194, 0.5744650565997773128, 0.5764597269351932063, 0.5784543972706092108, 0.5804490676060251042, 0.5824437379414409977, 0.5844384082768567801, 0.5864330786122726735, 0.5884277489476885670, 0.5904224192831044604, 0.5924170896185204649, 0.5944117599539363583, 0.5964064302893522518, 0.5984011006247680342, 0.6003957709601839277, 0.6023904412955998211, 0.6043851116310157146, 0.6063797819664317190, 0.6083744523018476125, 0.6103691226372635059, 0.6123637929726792883, 0.6143584633080951818, 0.6163531336435110752, 0.6183478039789269687, 0.6203424743143429732, 0.6223371446497588666, 0.6243318149851747600, 0.6263264853205905425, 0.6283211556560064359, 0.6303158259914223294, 0.6323104963268382228, 0.6343051666622542273, 0.6362998369976701207, 0.6382945073330860142, 0.6402891776685017966, 0.6422838480039176901, 0.6442785183393335835, 0.6462731886747494769, 0.6482678590101653704, 0.6502625293455813749, 0.6522571996809972683, 0.6542518700164131618, 0.6562465403518289442, 0.6582412106872448376, 0.6602358810226607311, 0.6622305513580766245, 0.6642252216934926290, 0.6662198920289085224, 0.6682145623643244159, 0.6702092326997401983, 0.6722039030351560918, 0.6741985733705719852, 0.6761932437059878787, 0.6781879140414038831, 0.6801825843768197766, 0.6821772547122356700, 0.6841719250476514524, 0.6861665953830673459, 0.6881612657184832393, 0.6901559360538991328, 0.6921506063893151373, 0.6941452767247310307, 0.6961399470601469242, 0.6981346173955627066, 0.7001292877309786000, 0.7021239580663944935, 0.7041186284018103869, 0.7061132987372263914, 0.7081079690726422848, 0.7101026394080581783, 0.7120973097434739607, 0.7140919800788898542, 0.7160866504143057476, 0.7180813207497216411, 0.7200759910851376455, 0.7220706614205535390, 0.7240653317559694324, 0.7260600020913853259, 0.7280546724268011083, 0.7300493427622170017, 0.7320440130976328952, 0.7340386834330488997, 0.7360333537684647931, 0.7380280241038806865, 0.7400226944392965800, 0.7420173647747123624, 0.7440120351101282559, 0.7460067054455441493, 0.7480013757809600428, 0.7499960461163760472, 0.7519907164517919407, 0.7539853867872078341, 0.7559800571226236166, 0.7579747274580395100, 0.7599693977934554034, 0.7619640681288712969, 0.7639587384642873014, 0.7659534087997031948, 0.7679480791351190883, 0.7699427494705348707, 0.7719374198059507641, 0.7739320901413666576, 0.7759267604767825510, 0.7779214308121985555, 0.7799161011476144489, 0.7819107714830303424, 0.7839054418184462358, 0.7859001121538620183, 0.7878947824892779117, 0.7898894528246938052, 0.7918841231601098096, 0.7938787934955257031, 0.7958734638309415965, 0.7978681341663574900, 0.7998628045017732724, 0.8018574748371891658, 0.8038521451726050593, 0.8058468155080210638, 0.8078414858434369572, 0.8098361561788528507, 0.8118308265142687441, 0.8138254968496845265, 0.8158201671851004200, 0.8178148375205163134, 0.8198095078559323179, 0.8218041781913482113, 0.8237988485267641048, 0.8257935188621799982, 0.8277881891975957807, 0.8297828595330116741, 0.8317775298684275675, 0.8337722002038435720, 0.8357668705392594655, 0.8377615408746753589, 0.8397562112100912524, 0.8417508815455070348, 0.8437455518809229282, 0.8457402222163388217, 0.8477348925517547151, 0.8497295628871707196, 0.8517242332225866130, 0.8537189035580025065, 0.8557135738934183999, 0.8577082442288341824, 0.8597029145642500758, 0.8616975848996659693, 0.8636922552350819737, 0.8656869255704978672, 0.8676815959059137606, 0.8696762662413296541, 0.8716709365767454365, 0.8736656069121613299, 0.8756602772475772234, 0.8776549475829932279, 0.8796496179184091213, 0.8816442882538250148, 0.8836389585892409082, 0.8856336289246566906, 0.8876282992600725841, 0.8896229695954884775, 0.8916176399309044820, 0.8936123102663203754, 0.8956069806017362689, 0.8976016509371521623, 0.8995963212725679448, 0.9015909916079838382, 0.9035856619433997317, 0.9055803322788157361, 0.9075750026142316296, 0.9095696729496475230, 0.9115643432850634165, 0.9135590136204791989, 0.9155536839558950923, 0.9175483542913109858, 0.9195430246267269903, 0.9215376949621428837, 0.9235323652975587772, 0.9255270356329746706, 0.9275217059683905640, 0.9295163763038063465, 0.9315110466392222399, 0.9335057169746382444, 0.9355003873100541378, 0.9374950576454700313, 0.9394897279808859247, 0.9414843983163018182, 0.9434790686517176006, 0.9454737389871334940, 0.9474684093225493875, 0.9494630796579653920, 0.9514577499933812854, 0.9534524203287971789, 0.9554470906642130723, 0.9574417609996288547, 0.9594364313350447482, 0.9614311016704606416, 0.9634257720058766461, 0.9654204423412925395, 0.9674151126767084330, 0.9694097830121243264, 0.9714044533475401089, 0.9733991236829560023, 0.9753937940183718958, 0.9773884643537879002, 0.9793831346892037937, 0.9813778050246196871, 0.9833724753600355806, 0.9853671456954513630, 0.9873618160308672564, 0.9892257831175960137 ),
 .UNSPECIFIED. ) 
 CURVE ( )  GEOMETRIC_REPRESENTATION_ITEM ( )  RATIONAL_B_SPLINE_CURVE ( ( 1.000000000000000000, 0.9807852804032304306, 1.000000000000000000, 0.9807852804032304306, 1.000000000000000000, 0.9807852804032304306, 1.000000000000000000, 0.9807852804032304306, 1.000000000000000000, 0.9807852804032304306, 1.000000000000000000, 0.9807852804032304306, 1.000000000000000000, 0.9807852804032304306, 1.000000000000000000, 0.9807852804032304306, 1.000000000000000000, 0.9807852804032304306, 1.000000000000000000, 0.9807852804032304306, 1.000000000000000000, 0.9807852804032304306, 1.000000000000000000, 0.9807852804032304306, 1.000000000000000000, 0.9807852804032304306, 1.000000000000000000, 0.9807852804032304306, 1.000000000000000000, 0.9807852804032304306, 1.000000000000000000, 0.9807852804032304306, 1.000000000000000000, 0.9807852804032304306, 1.000000000000000000, 0.9807852804032304306, 1.000000000000000000, 0.9807852804032304306, 1.000000000000000000, 0.9807852804032304306, 1.000000000000000000, 0.9807852804032304306, 1.000000000000000000, 0.9807852804032304306, 1.000000000000000000, 0.9807852804032304306, 1.000000000000000000, 0.9807852804032304306, 1.000000000000000000, 0.9807852804032304306, 1.000000000000000000, 0.9807852804032304306, 1.000000000000000000, 0.9807852804032304306, 1.000000000000000000, 0.9807852804032304306, 1.000000000000000000, 0.9807852804032304306, 1.000000000000000000, 0.9807852804032304306, 1.000000000000000000, 0.9807852804032304306, 1.000000000000000000, 0.9807852804032304306, 1.000000000000000000, 0.9807852804032304306, 1.000000000000000000, 0.9807852804032304306, 1.000000000000000000, 0.9807852804032304306, 1.000000000000000000, 0.9807852804032304306, 1.000000000000000000, 0.9807852804032304306, 1.000000000000000000, 0.9807852804032304306, 1.000000000000000000, 0.9807852804032304306, 1.000000000000000000, 0.9807852804032304306, 1.000000000000000000, 0.9807852804032304306, 1.000000000000000000, 0.9807852804032304306, 1.000000000000000000, 0.9807852804032304306, 1.000000000000000000, 0.9807852804032304306, 1.000000000000000000, 0.9807852804032304306, 1.000000000000000000, 0.9807852804032304306, 1.000000000000000000, 0.9807852804032304306, 1.000000000000000000, 0.9807852804032304306, 1.000000000000000000, 0.9807852804032304306, 1.000000000000000000, 0.9807852804032304306, 1.000000000000000000, 0.9807852804032304306, 1.000000000000000000, 0.9807852804032304306, 1.000000000000000000, 0.9807852804032304306, 1.000000000000000000, 0.9807852804032304306, 1.000000000000000000, 0.9807852804032304306, 1.000000000000000000, 0.9807852804032304306, 1.000000000000000000, 0.9807852804032304306, 1.000000000000000000, 0.9807852804032304306, 1.000000000000000000, 0.9807852804032304306, 1.000000000000000000, 0.9807852804032304306, 1.000000000000000000, 0.9807852804032304306, 1.000000000000000000, 0.9807852804032304306, 1.000000000000000000, 0.9807852804032304306, 1.000000000000000000, 0.9807852804032304306, 1.000000000000000000, 0.9807852804032304306, 1.000000000000000000, 0.9807852804032304306, 1.000000000000000000, 0.9807852804032304306, 1.000000000000000000, 0.9807852804032304306, 1.000000000000000000, 0.9807852804032304306, 1.000000000000000000, 0.9807852804032304306, 1.000000000000000000, 0.9807852804032304306, 1.000000000000000000, 0.9807852804032304306, 1.000000000000000000, 0.9807852804032304306, 1.000000000000000000, 0.9807852804032304306, 1.000000000000000000, 0.9807852804032304306, 1.000000000000000000, 0.9807852804032304306, 1.000000000000000000, 0.9807852804032304306, 1.000000000000000000, 0.9807852804032304306, 1.000000000000000000, 0.9807852804032304306, 1.000000000000000000, 0.9807852804032304306, 1.000000000000000000, 0.9807852804032304306, 1.000000000000000000, 0.9807852804032304306, 1.000000000000000000, 0.9807852804032304306, 1.000000000000000000, 0.9807852804032304306, 1.000000000000000000, 0.9807852804032304306, 1.000000000000000000, 0.9807852804032304306, 1.000000000000000000, 0.9807852804032304306, 1.000000000000000000, 0.9807852804032304306, 1.000000000000000000, 0.9807852804032304306, 1.000000000000000000, 0.9807852804032304306, 1.000000000000000000, 0.9807852804032304306, 1.000000000000000000, 0.9807852804032304306, 1.000000000000000000, 0.9807852804032304306, 1.000000000000000000, 0.9807852804032304306, 1.000000000000000000, 0.9807852804032304306, 1.000000000000000000, 0.9807852804032304306, 1.000000000000000000, 0.9807852804032304306, 1.000000000000000000, 0.9807852804032304306, 1.000000000000000000, 0.9807852804032304306, 1.000000000000000000, 0.9807852804032304306, 1.000000000000000000, 0.9807852804032304306, 1.000000000000000000, 0.9807852804032304306, 1.000000000000000000, 0.9807852804032304306, 1.000000000000000000, 0.9807852804032304306, 1.000000000000000000, 0.9807852804032304306, 1.000000000000000000, 0.9807852804032304306, 1.000000000000000000, 0.9807852804032304306, 1.000000000000000000, 0.9807852804032304306, 1.000000000000000000, 0.9807852804032304306, 1.000000000000000000, 0.9807852804032304306, 1.000000000000000000, 0.9807852804032304306, 1.000000000000000000, 0.9807852804032304306, 1.000000000000000000, 0.9807852804032304306, 1.000000000000000000, 0.9807852804032304306, 1.000000000000000000, 0.9807852804032304306, 1.000000000000000000, 0.9807852804032304306, 1.000000000000000000, 0.9807852804032304306, 1.000000000000000000, 0.9807852804032304306, 1.000000000000000000, 0.9807852804032304306, 1.000000000000000000, 0.9807852804032304306, 1.000000000000000000, 0.9807852804032304306, 1.000000000000000000, 0.9807852804032304306, 1.000000000000000000, 0.9807852804032304306, 1.000000000000000000, 0.9807852804032304306, 1.000000000000000000, 0.9807852804032304306, 1.000000000000000000, 0.9807852804032304306, 1.000000000000000000, 0.9807852804032304306, 1.000000000000000000, 0.9807852804032304306, 1.000000000000000000, 0.9807852804032304306, 1.000000000000000000, 0.9807852804032304306, 1.000000000000000000, 0.9807852804032304306, 1.000000000000000000, 0.9807852804032304306, 1.000000000000000000, 0.9807852804032304306, 1.000000000000000000, 0.9807852804032304306, 1.000000000000000000, 0.9807852804032304306, 1.000000000000000000, 0.9807852804032304306, 1.000000000000000000, 0.9807852804032304306, 1.000000000000000000, 0.9807852804032304306, 1.000000000000000000, 0.9807852804032304306, 1.000000000000000000, 0.9807852804032304306, 1.000000000000000000, 0.9807852804032304306, 1.000000000000000000, 0.9807852804032304306, 1.000000000000000000, 0.9807852804032304306, 1.000000000000000000, 0.9807852804032304306, 1.000000000000000000, 0.9807852804032304306, 1.000000000000000000, 0.9807852804032304306, 1.000000000000000000, 0.9807852804032304306, 1.000000000000000000, 0.9807852804032304306, 1.000000000000000000, 0.9807852804032304306, 1.000000000000000000, 0.9807852804032304306, 1.000000000000000000, 0.9807852804032304306, 1.000000000000000000, 0.9807852804032304306, 1.000000000000000000, 0.9807852804032304306, 1.000000000000000000, 0.9807852804032304306, 1.000000000000000000, 0.9807852804032304306, 1.000000000000000000, 0.9807852804032304306, 1.000000000000000000, 0.9807852804032304306, 1.000000000000000000, 0.9807852804032304306, 1.000000000000000000, 0.9807852804032304306, 1.000000000000000000, 0.9807852804032304306, 1.000000000000000000, 0.9807852804032304306, 1.000000000000000000, 0.9807852804032304306, 1.000000000000000000, 0.9807852804032304306, 1.000000000000000000, 0.9807852804032304306, 1.000000000000000000, 0.9807852804032304306, 1.000000000000000000, 0.9807852804032304306, 1.000000000000000000, 0.9807852804032304306, 1.000000000000000000, 0.9807852804032304306, 1.000000000000000000, 0.9807852804032304306, 1.000000000000000000, 0.9807852804032304306, 1.000000000000000000, 0.9807852804032304306, 1.000000000000000000, 0.9807852804032304306, 1.000000000000000000, 0.9807852804032304306, 1.000000000000000000, 0.9807852804032304306, 1.000000000000000000, 0.9807852804032304306, 1.000000000000000000, 0.9807852804032304306, 1.000000000000000000, 0.9807852804032304306, 1.000000000000000000, 0.9807852804032304306, 1.000000000000000000, 0.9807852804032304306, 1.000000000000000000, 0.9807852804032304306, 1.000000000000000000, 0.9807852804032304306, 1.000000000000000000, 0.9807852804032304306, 1.000000000000000000, 0.9807852804032304306, 1.000000000000000000, 0.9807852804032304306, 1.000000000000000000, 0.9807852804032304306, 1.000000000000000000, 0.9807852804032304306, 1.000000000000000000, 0.9807852804032304306, 1.000000000000000000, 0.9807852804032304306, 1.000000000000000000, 0.9807852804032304306, 1.000000000000000000, 0.9807852804032304306, 1.000000000000000000, 0.9807852804032304306, 1.000000000000000000, 0.9807852804032304306, 1.000000000000000000, 0.9807852804032304306, 1.000000000000000000, 0.9807852804032304306, 1.000000000000000000, 0.9807852804032304306, 1.000000000000000000, 0.9807852804032304306, 1.000000000000000000, 0.9807852804032304306, 1.000000000000000000, 0.9807852804032304306, 1.000000000000000000, 0.9807852804032304306, 1.000000000000000000, 0.9807852804032304306, 1.000000000000000000, 0.9807852804032304306, 1.000000000000000000, 0.9807852804032304306, 1.000000000000000000, 0.9807852804032304306, 1.000000000000000000, 0.9807852804032304306, 1.000000000000000000, 0.9807852804032304306, 1.000000000000000000, 0.9807852804032304306, 1.000000000000000000, 0.9807852804032304306, 1.000000000000000000, 0.9807852804032304306, 1.000000000000000000, 0.9807852804032304306, 1.000000000000000000, 0.9807852804032304306, 1.000000000000000000, 0.9807852804032304306, 1.000000000000000000, 0.9807852804032304306, 1.000000000000000000, 0.9807852804032304306, 1.000000000000000000, 0.9807852804032304306, 1.000000000000000000, 0.9807852804032304306, 1.000000000000000000, 0.9807852804032304306, 1.000000000000000000, 0.9807852804032304306, 1.000000000000000000, 0.9807852804032304306, 1.000000000000000000, 0.9807852804032304306, 1.000000000000000000, 0.9807852804032304306, 1.000000000000000000, 0.9807852804032304306, 1.000000000000000000, 0.9807852804032304306, 1.000000000000000000, 0.9807852804032304306, 1.000000000000000000, 0.9807852804032304306, 1.000000000000000000, 0.9807852804032304306, 1.000000000000000000, 0.9807852804032304306, 1.000000000000000000, 0.9807852804032304306, 1.000000000000000000, 0.9807852804032304306, 1.000000000000000000, 0.9807852804032304306, 1.000000000000000000, 0.9807852804032304306, 1.000000000000000000, 0.9807852804032304306, 1.000000000000000000, 0.9807852804032304306, 1.000000000000000000, 0.9807852804032304306, 1.000000000000000000, 0.9807852804032304306, 1.000000000000000000, 0.9807852804032304306, 1.000000000000000000, 0.9807852804032304306, 1.000000000000000000, 0.9807852804032304306, 1.000000000000000000, 0.9807852804032304306, 1.000000000000000000, 0.9807852804032304306, 1.000000000000000000, 0.9807852804032304306, 1.000000000000000000, 0.9807852804032304306, 1.000000000000000000, 0.9807852804032304306, 1.000000000000000000, 0.9807852804032304306, 1.000000000000000000, 0.9807852804032304306, 1.000000000000000000, 0.9807852804032304306, 1.000000000000000000, 0.9807852804032304306, 1.000000000000000000, 0.9807852804032304306, 1.000000000000000000, 0.9807852804032304306, 1.000000000000000000, 0.9807852804032304306, 1.000000000000000000, 0.9807852804032304306, 1.000000000000000000, 0.9807852804032304306, 1.000000000000000000, 0.9807852804032304306, 1.000000000000000000, 0.9807852804032304306, 1.000000000000000000, 0.9807852804032304306, 1.000000000000000000, 0.9807852804032304306, 1.000000000000000000, 0.9807852804032304306, 1.000000000000000000, 0.9807852804032304306, 1.000000000000000000, 0.9807852804032304306, 1.000000000000000000, 0.9807852804032304306, 1.000000000000000000, 0.9807852804032304306, 1.000000000000000000, 0.9807852804032304306, 1.000000000000000000, 0.9807852804032304306, 1.000000000000000000, 0.9807852804032304306, 1.000000000000000000, 0.9807852804032304306, 1.000000000000000000, 0.9807852804032304306, 1.000000000000000000, 0.9807852804032304306, 1.000000000000000000, 0.9807852804032304306, 1.000000000000000000, 0.9807852804032304306, 1.000000000000000000, 0.9807852804032304306, 1.000000000000000000, 0.9807852804032304306, 1.000000000000000000, 0.9807852804032304306, 1.000000000000000000, 0.9807852804032304306, 1.000000000000000000, 0.9807852804032304306, 1.000000000000000000, 0.9807852804032304306, 1.000000000000000000, 0.9807852804032304306, 1.000000000000000000, 0.9807852804032304306, 1.000000000000000000, 0.9807852804032304306, 1.000000000000000000, 0.9807852804032304306, 1.000000000000000000, 0.9807852804032304306, 1.000000000000000000, 0.9807852804032304306, 1.000000000000000000, 0.9807852804032304306, 1.000000000000000000, 0.9807852804032304306, 1.000000000000000000, 0.9807852804032304306, 1.000000000000000000, 0.9807852804032304306, 1.000000000000000000, 0.9807852804032304306, 1.000000000000000000, 0.9807852804032304306, 1.000000000000000000, 0.9807852804032304306, 1.000000000000000000, 0.9807852804032304306, 1.000000000000000000, 0.9807852804032304306, 1.000000000000000000, 0.9807852804032304306, 1.000000000000000000, 0.9807852804032304306, 1.000000000000000000, 0.9807852804032304306, 1.000000000000000000, 0.9807852804032304306, 1.000000000000000000, 0.9807852804032304306, 1.000000000000000000, 0.9807852804032304306, 1.000000000000000000, 0.9807852804032304306, 1.000000000000000000, 0.9807852804032304306, 1.000000000000000000, 0.9807852804032304306, 1.000000000000000000, 0.9807852804032304306, 1.000000000000000000, 0.9807852804032304306, 1.000000000000000000, 0.9807852804032304306, 1.000000000000000000, 0.9807852804032304306, 1.000000000000000000, 0.9807852804032304306, 1.000000000000000000, 0.9807852804032304306, 1.000000000000000000, 0.9807852804032304306, 1.000000000000000000, 0.9807852804032304306, 1.000000000000000000, 0.9807852804032304306, 1.000000000000000000, 0.9807852804032304306, 1.000000000000000000, 0.9807852804032304306, 1.000000000000000000, 0.9807852804032304306, 1.000000000000000000, 0.9807852804032304306, 1.000000000000000000, 0.9807852804032304306, 1.000000000000000000, 0.9807852804032304306, 1.000000000000000000, 0.9807852804032304306, 1.000000000000000000, 0.9807852804032304306, 1.000000000000000000, 0.9807852804032304306, 1.000000000000000000, 0.9807852804032304306, 1.000000000000000000, 0.9807852804032304306, 1.000000000000000000, 0.9807852804032304306, 1.000000000000000000, 0.9807852804032304306, 1.000000000000000000, 0.9807852804032304306, 1.000000000000000000, 0.9807852804032304306, 1.000000000000000000, 0.9807852804032304306, 1.000000000000000000, 0.9807852804032304306, 1.000000000000000000, 0.9807852804032304306, 1.000000000000000000, 0.9807852804032304306, 1.000000000000000000, 0.9807852804032304306, 1.000000000000000000, 0.9807852804032304306, 1.000000000000000000, 0.9807852804032304306, 1.000000000000000000, 0.9807852804032304306, 1.000000000000000000, 0.9807852804032304306, 1.000000000000000000, 0.9807852804032304306, 1.000000000000000000, 0.9807852804032304306, 1.000000000000000000, 0.9807852804032304306, 1.000000000000000000, 0.9807852804032304306, 1.000000000000000000, 0.9807852804032304306, 1.000000000000000000, 0.9807852804032304306, 1.000000000000000000, 0.9807852804032304306, 1.000000000000000000, 0.9807852804032304306, 1.000000000000000000, 0.9807852804032304306, 1.000000000000000000, 0.9807852804032304306, 1.000000000000000000, 0.9807852804032304306, 1.000000000000000000, 0.9807852804032304306, 1.000000000000000000, 0.9807852804032304306, 1.000000000000000000, 0.9807852804032304306, 1.000000000000000000, 0.9807852804032304306, 1.000000000000000000, 0.9807852804032304306, 1.000000000000000000, 0.9807852804032304306, 1.000000000000000000, 0.9807852804032304306, 1.000000000000000000, 0.9807852804032304306, 1.000000000000000000, 0.9807852804032304306, 1.000000000000000000, 0.9807852804032304306, 1.000000000000000000, 0.9807852804032304306, 1.000000000000000000, 0.9807852804032304306, 1.000000000000000000, 0.9807852804032304306, 1.000000000000000000, 0.9807852804032304306, 1.000000000000000000, 0.9807852804032304306, 1.000000000000000000, 0.9807852804032304306, 1.000000000000000000, 0.9807852804032304306, 1.000000000000000000, 0.9807852804032304306, 1.000000000000000000, 0.9807852804032304306, 1.000000000000000000, 0.9807852804032304306, 1.000000000000000000, 0.9807852804032304306, 1.000000000000000000, 0.9807852804032304306, 1.000000000000000000, 0.9807852804032304306, 1.000000000000000000, 0.9807852804032304306, 1.000000000000000000, 0.9807852804032304306, 1.000000000000000000, 0.9807852804032304306, 1.000000000000000000, 0.9807852804032304306, 1.000000000000000000, 0.9807852804032304306, 1.000000000000000000, 0.9807852804032304306, 1.000000000000000000, 0.9807852804032304306, 1.000000000000000000, 0.9807852804032304306, 1.000000000000000000, 0.9807852804032304306, 1.000000000000000000, 0.9807852804032304306, 1.000000000000000000, 0.9807852804032304306, 1.000000000000000000, 0.9807852804032304306, 1.000000000000000000, 0.9807852804032304306, 1.000000000000000000, 0.9807852804032304306, 1.000000000000000000, 0.9807852804032304306, 1.000000000000000000, 0.9807852804032304306, 1.000000000000000000, 0.9807852804032304306, 1.000000000000000000, 0.9807852804032304306, 1.000000000000000000, 0.9807852804032304306, 1.000000000000000000, 0.9807852804032304306, 1.000000000000000000, 0.9807852804032304306, 1.000000000000000000, 0.9807852804032304306, 1.000000000000000000, 0.9807852804032304306, 1.000000000000000000, 0.9807852804032304306, 1.000000000000000000, 0.9807852804032304306, 1.000000000000000000, 0.9807852804032304306, 1.000000000000000000, 0.9807852804032304306, 1.000000000000000000, 0.9807852804032304306, 1.000000000000000000, 0.9807852804032304306, 1.000000000000000000, 0.9807852804032304306, 1.000000000000000000, 0.9807852804032304306, 1.000000000000000000, 0.9807852804032304306, 1.000000000000000000, 0.9807852804032304306, 1.000000000000000000, 0.9807852804032304306, 1.000000000000000000, 0.9807852804032304306, 1.000000000000000000, 0.9807852804032304306, 1.000000000000000000, 0.9807852804032304306, 1.000000000000000000, 0.9807852804032304306, 1.000000000000000000, 0.9807852804032304306, 1.000000000000000000, 0.9807852804032304306, 1.000000000000000000, 0.9807852804032304306, 1.000000000000000000, 0.9807852804032304306, 1.000000000000000000, 0.9807852804032304306, 1.000000000000000000, 0.9807852804032304306, 1.000000000000000000, 0.9807852804032304306, 1.000000000000000000, 0.9807852804032304306, 1.000000000000000000, 0.9807852804032304306, 1.000000000000000000, 0.9807852804032304306, 1.000000000000000000, 0.9807852804032304306, 1.000000000000000000, 0.9807852804032304306, 1.000000000000000000, 0.9807852804032304306, 1.000000000000000000, 0.9807852804032304306, 1.000000000000000000, 0.9807852804032304306, 1.000000000000000000, 0.9807852804032304306, 1.000000000000000000, 0.9807852804032304306, 1.000000000000000000, 0.9807852804032304306, 1.000000000000000000, 0.9807852804032304306, 1.000000000000000000, 0.9807852804032304306, 1.000000000000000000, 0.9807852804032304306, 1.000000000000000000, 0.9807852804032304306, 1.000000000000000000, 0.9807852804032304306, 1.000000000000000000, 0.9807852804032304306, 1.000000000000000000, 0.9807852804032304306, 1.000000000000000000, 0.9807852804032304306, 1.000000000000000000, 0.9807852804032304306, 1.000000000000000000, 0.9807852804032304306, 1.000000000000000000, 0.9807852804032304306, 1.000000000000000000, 0.9807852804032304306, 1.000000000000000000, 0.9807852804032304306, 1.000000000000000000, 0.9807852804032304306, 1.000000000000000000, 0.9807852804032304306, 1.000000000000000000, 0.9807852804032304306, 1.000000000000000000, 0.9807852804032304306, 1.000000000000000000, 0.9807852804032304306, 1.000000000000000000, 0.9807852804032304306, 1.000000000000000000, 0.9807852804032304306, 1.000000000000000000, 0.9807852804032304306, 1.000000000000000000, 0.9807852804032304306, 1.000000000000000000, 0.9807852804032304306, 1.000000000000000000, 0.9807852804032304306, 1.000000000000000000, 0.9807852804032304306, 1.000000000000000000, 0.9807852804032304306, 1.000000000000000000, 0.9807852804032304306, 1.000000000000000000, 0.9807852804032304306, 1.000000000000000000, 0.9807852804032304306, 1.000000000000000000, 0.9807852804032304306, 1.000000000000000000, 0.9807852804032304306, 1.000000000000000000, 0.9807852804032304306, 1.000000000000000000, 0.9807852804032304306, 1.000000000000000000, 0.9807852804032304306, 1.000000000000000000, 0.9807852804032304306, 1.000000000000000000, 0.9807852804032304306, 1.000000000000000000, 0.9807852804032304306, 1.000000000000000000, 0.9807852804032304306, 1.000000000000000000, 0.9807852804032304306, 1.000000000000000000, 0.9807852804032304306, 1.000000000000000000, 0.9807852804032304306, 1.000000000000000000, 0.9807852804032304306, 1.000000000000000000, 0.9807852804032304306, 1.000000000000000000, 0.9807852804032304306, 1.000000000000000000, 0.9807852804032304306, 1.000000000000000000, 0.9807852804032304306, 1.000000000000000000, 0.9807852804032304306, 1.000000000000000000, 0.9807852804032304306, 1.000000000000000000, 0.9807852804032304306, 1.000000000000000000, 0.9807852804032304306, 1.000000000000000000, 0.9807852804032304306, 1.000000000000000000, 0.9807852804032304306, 1.000000000000000000, 0.9807852804032304306, 1.000000000000000000, 0.9807852804032304306, 1.000000000000000000, 0.9807852804032304306, 1.000000000000000000, 0.9807852804032304306, 1.000000000000000000, 0.9807852804032304306, 1.000000000000000000, 0.9807852804032304306, 1.000000000000000000, 0.9807852804032304306, 1.000000000000000000, 0.9807852804032304306, 1.000000000000000000, 0.9807852804032304306, 1.000000000000000000, 0.9807852804032304306, 1.000000000000000000, 0.9807852804032304306, 1.000000000000000000, 0.9807852804032304306, 1.000000000000000000, 0.9807852804032304306, 1.000000000000000000, 0.9807852804032304306, 1.000000000000000000, 0.9807852804032304306, 1.000000000000000000, 0.9807852804032304306, 1.000000000000000000, 0.9807852804032304306, 1.000000000000000000, 0.9807852804032304306, 1.000000000000000000, 0.9807852804032304306, 1.000000000000000000, 0.9807852804032304306, 1.000000000000000000, 0.9807852804032304306, 1.000000000000000000, 0.9807852804032304306, 1.000000000000000000, 0.9820443487461643084, 0.9976468673449425673 ) ) 
 REPRESENTATION_ITEM ( '' )  );
#12233 = CARTESIAN_POINT ( 'NONE',  ( -40.53162694259544452, 396.6198905683720568, 11.84573899990672885 ) ) ;
#12234 = CARTESIAN_POINT ( 'NONE',  ( -8.685887942688735208, 482.2448905601784759, -2.449293598294705724E-15 ) ) ;
#12235 = DIRECTION ( 'NONE',  ( 1.191790137725560488E-16, -1.000000000000000000, 0.000000000000000000 ) ) ;
#12236 = DIRECTION ( 'NONE',  ( 0.000000000000000000, 0.000000000000000000, -1.000000000000000000 ) ) ;
#12237 = CARTESIAN_POINT ( 'NONE',  ( -16.84014894278198327, 311.6198905683720000, -11.84573899990672707 ) ) ;
#12238 = CARTESIAN_POINT ( 'NONE',  ( -35.09675569278796559, 465.7448905683720568, 15.47720386886985366 ) ) ;
#12239 = ORIENTED_EDGE ( 'NONE', *, *, #21176, .T. ) ;
#12240 = CARTESIAN_POINT ( 'NONE',  ( -11.73070664223726212, 463.1823905601784759, -11.32908994701042715 ) ) ;
#12241 = CARTESIAN_POINT ( 'NONE',  ( -19.19641293061497578, 287.3073905683720000, 14.20200298773971426 ) ) ;
#12242 = VECTOR ( 'NONE', #10392, 1000.000000000000000 ) ;
#12243 = ORIENTED_EDGE ( 'NONE', *, *, #10480, .T. ) ;
#12244 = CARTESIAN_POINT ( 'NONE',  ( -11.93348319268872970, 440.0573905683720000, 3.332260488124728859 ) ) ;
#12245 = EDGE_LOOP ( 'NONE', ( #981, #83, #13037, #13039 ) ) ;
#12246 = DIRECTION ( 'NONE',  ( 0.000000000000000000, 0.000000000000000000, 1.000000000000000000 ) ) ;
#12247 = CARTESIAN_POINT ( 'NONE',  ( -35.09675569278794427, 305.7448905683720568, 15.47720386886985366 ) ) ;
#12248 = CARTESIAN_POINT ( 'NONE',  ( -42.88789093042843348, 376.3073905683720000, 9.489475012073734561 ) ) ;
#12249 = CARTESIAN_POINT ( 'NONE',  ( -14.54375231895777176, 373.4948905601784759, -14.14213562373094746 ) ) ;
#12250 = CARTESIAN_POINT ( 'NONE',  ( -48.68588794268872988, 531.6823905765655809, -3.978247347593158345 ) ) ;
#12251 = CARTESIAN_POINT ( 'NONE',  ( -38.17536295476245556, 395.4323905683720000, 14.20200298773971781 ) ) ;
#12252 = CARTESIAN_POINT ( 'NONE',  ( -40.53162694259542320, 234.1198905683720000, -11.84573899990672707 ) ) ;
#12253 = CARTESIAN_POINT ( 'NONE',  ( -14.48388495494900852, 429.8073905683720000, -9.489475012073734561 ) ) ;
#12254 = CARTESIAN_POINT ( 'NONE',  ( -24.70764059509556176, 349.1823905765655809, -19.99999999999999289 ) ) ;
#12255 = CARTESIAN_POINT ( 'NONE',  ( -28.68588794268872633, 378.8848358243226357, -20.00000000000000000 ) ) ;
#12256 = CARTESIAN_POINT ( 'NONE',  ( -11.93348319268871371, 298.5573905683720000, 3.332260488124728859 ) ) ;
#12257 = CARTESIAN_POINT ( 'NONE',  ( -22.27502019258949773, 482.2448905683720568, -15.47720386886985544 ) ) ;
#12258 = CARTESIAN_POINT ( 'NONE',  ( -8.685887942689062058, 516.6823905765653535, 3.978247347593932837 ) ) ;
#12259 = DIRECTION ( 'NONE',  ( 0.000000000000000000, 0.000000000000000000, 1.000000000000000000 ) ) ;
#12260 = CARTESIAN_POINT ( 'NONE',  ( -24.70764059509555111, 304.4323905601784759, -19.99999999999999289 ) ) ;
#12261 = ADVANCED_FACE ( 'NONE', ( #5855 ), #12617, .T. ) ;
#12262 = CARTESIAN_POINT ( 'NONE',  ( -40.53162694259544452, 396.6198905683720568, 11.84573899990672885 ) ) ;
#12263 = CARTESIAN_POINT ( 'NONE',  ( 65.85920792673738333, 160.1716627696692683, 40.00000000000000000 ) ) ;
#12264 = CARTESIAN_POINT ( 'NONE',  ( -8.685887942688744090, 532.5573905601784190, -3.978247347593165895 ) ) ;
#12265 = CARTESIAN_POINT ( 'NONE',  ( -38.17536295476244845, 345.4323905683719431, 14.20200298773971781 ) ) ;
#12266 = ORIENTED_EDGE ( 'NONE', *, *, #9956, .T. ) ;
#12267 = CARTESIAN_POINT ( 'NONE',  ( -44.16309181155858710, 503.2448905683719431, -6.410867750099231266 ) ) ;
#12268 = ORIENTED_EDGE ( 'NONE', *, *, #12310, .T. ) ;
#12269 = CARTESIAN_POINT ( 'NONE',  ( -28.68588794268871567, 354.7448905601784759, -19.99999999999999289 ) ) ;
#12270 = CARTESIAN_POINT ( 'NONE',  ( -48.68588794268870856, 381.9948905765655809, 0.000000000000000000 ) ) ;
#12271 = FACE_BOUND ( 'NONE', #5391, .T. ) ;
#12272 = ADVANCED_FACE ( 'NONE', ( #19438, #14587 ), #6234, .F. ) ;
#12273 = VECTOR ( 'NONE', #8, 1000.000000000000000 ) ;
#12274 = CARTESIAN_POINT ( 'NONE',  ( -18.68588794268873698, 323.8848358243226357, -20.00000000000000355 ) ) ;
#12275 = CARTESIAN_POINT ( 'NONE',  ( -21.03221929538694468, 518.8698905765655809, -18.47759065022572855 ) ) ;
#12276 = CARTESIAN_POINT ( 'NONE',  ( -16.84014894278199748, 457.6198905683720568, 11.84573899990672530 ) ) ;
#12277 = ORIENTED_EDGE ( 'NONE', *, *, #17868, .T. ) ;
#12278 = CARTESIAN_POINT ( 'NONE',  ( -25.35362745456399480, 486.6823905683721136, 16.75240474999998952 ) ) ;
#12279 = CARTESIAN_POINT ( 'NONE',  ( 62.02695467647412642, 160.1716627696692683, 61.71700053422265597 ) ) ;
#12280 = CARTESIAN_POINT ( 'NONE',  ( -24.70764059509556532, 399.1823905765656377, -19.99999999999999289 ) ) ;
#12281 = CARTESIAN_POINT ( 'NONE',  ( -10.20829729246299955, 476.3698905765656377, 7.653668647301790529 ) ) ;
#12282 = CYLINDRICAL_SURFACE ( 'NONE', #21313, 19.99999999999999645 ) ;
#12283 = CARTESIAN_POINT ( 'NONE',  ( -8.685887942688605534, 482.5573905601784190, -3.978247347592846594 ) ) ;
#12284 = DIRECTION ( 'NONE',  ( -1.000000000000000000, 0.000000000000000000, 0.000000000000000000 ) ) ;
#12285 = CARTESIAN_POINT ( 'NONE',  ( 51.98438129372387806, 56.85652257517428865, 94.99999999999994316 ) ) ;
#12286 = DIRECTION ( 'NONE',  ( 0.000000000000000000, 0.000000000000000000, 1.000000000000000000 ) ) ;
#12287 = CYLINDRICAL_SURFACE ( 'NONE', #5212, 15.00000000000000000 ) ;
#12288 = CARTESIAN_POINT ( 'NONE',  ( -35.09675569278794427, 287.2448905683720000, 15.47720386886985366 ) ) ;
#12289 = CARTESIAN_POINT ( 'NONE',  ( -47.16347859291445133, 402.6198905765655809, 7.653668647301805628 ) ) ;
#12290 = CARTESIAN_POINT ( 'NONE',  ( -11.93348319268872970, 440.3698905683720000, -2.051577885510841163E-15 ) ) ;
#12291 = CARTESIAN_POINT ( 'NONE',  ( 51.50493485826542184, 141.8799693780962912, -20.00000000000000355 ) ) ;
#12292 = CARTESIAN_POINT ( 'NONE',  ( -22.27502019258946575, 278.4948905683720000, 15.47720386886985189 ) ) ;
#12293 = ORIENTED_EDGE ( 'NONE', *, *, #3720, .F. ) ;
#12294 = CYLINDRICAL_SURFACE ( 'NONE', #20860, 19.99999999999999645 ) ;
#12295 = ORIENTED_EDGE ( 'NONE', *, *, #4148, .F. ) ;
#12296 = CARTESIAN_POINT ( 'NONE',  ( -19.19641293061499354, 488.8073905683720000, 14.20200298773971426 ) ) ;
#12297 = VERTEX_POINT ( 'NONE', #12847 ) ;
#12298 = CARTESIAN_POINT ( 'NONE',  ( -32.66413529028186957, 365.0573905601784190, -19.99999999999999289 ) ) ;
#12299 = CARTESIAN_POINT ( 'NONE',  ( -35.09675569278793716, 245.7448905683720000, 15.47720386886985366 ) ) ;
#12300 = VERTEX_POINT ( 'NONE', #3111 ) ;
#12301 = CARTESIAN_POINT ( 'NONE',  ( -28.68588794268872633, 174.3162933293988033, 20.00000000000000000 ) ) ;
#12302 = CARTESIAN_POINT ( 'NONE',  ( -36.33955658999052929, 453.8698905765656377, 18.47759065022572500 ) ) ;
#12303 = CARTESIAN_POINT ( 'NONE',  ( 5.074999999999999289, 0.000000000000000000, 0.000000000000000000 ) ) ;
#12304 = CARTESIAN_POINT ( 'NONE',  ( -48.68588794268872277, 457.2448905601784759, 0.000000000000000000 ) ) ;
#12305 = CARTESIAN_POINT ( 'NONE',  ( -45.43829269268869808, 225.0573905683720284, -3.332260488124726638 ) ) ;
#12306 = CARTESIAN_POINT ( 'NONE',  ( -40.53162694259545873, 526.6198905683720568, 11.84573899990672885 ) ) ;
#12307 = CARTESIAN_POINT ( 'NONE',  ( 60.03793209889851568, 30.52886280891152282, -136.1729372809869005 ) ) ;
#12308 = CARTESIAN_POINT ( 'NONE',  ( -16.84014894278197616, 240.1198905683720284, -11.84573899990672707 ) ) ;
#12309 = CARTESIAN_POINT ( 'NONE',  ( -11.93348319268871904, 330.6823905683721136, -3.332260488124732856 ) ) ;
#12310 = EDGE_CURVE ( 'NONE', #13961, #15268, #7347, .T. ) ;
#12311 = LINE ( 'NONE', #20640, #19228 ) ;
#12312 = CARTESIAN_POINT ( 'NONE',  ( -10.20829729246298534, 361.6198905601784759, 7.653668647301790529 ) ) ;
#12313 = VECTOR ( 'NONE', #18292, 1000.000000000000000 ) ;
#12314 = CARTESIAN_POINT ( 'NONE',  ( -44.16309181155857999, 393.2448905683720568, -6.410867750099231266 ) ) ;
#12315 = ADVANCED_FACE ( 'NONE', ( #3219 ), #11423, .T. ) ;
#12316 = LINE ( 'NONE', #7654, #15050 ) ;
#12317 = CARTESIAN_POINT ( 'NONE',  ( -24.70764059509556532, 384.4323905601784190, -19.99999999999999289 ) ) ;
#12318 = CIRCLE ( 'NONE', #18874, 6.500000000000000888 ) ;
#12319 = DIRECTION ( 'NONE',  ( -0.000000000000000000, -0.000000000000000000, -1.000000000000000000 ) ) ;
#12320 = VERTEX_POINT ( 'NONE', #11539 ) ;
#12321 = ORIENTED_EDGE ( 'NONE', *, *, #8792, .T. ) ;
#12322 = CARTESIAN_POINT ( 'NONE',  ( -16.84014894278200813, 511.6198905683720000, -11.84573899990672707 ) ) ;
#12323 = CARTESIAN_POINT ( 'NONE',  ( -28.68588794268872277, 378.8848358243226357, 38.00000000000000000 ) ) ;
#12324 = ORIENTED_EDGE ( 'NONE', *, *, #19928, .F. ) ;
#12325 = CARTESIAN_POINT ( 'NONE',  ( -19.19641293061497578, 311.9323905683720000, -14.20200298773971603 ) ) ;
#12326 = ORIENTED_EDGE ( 'NONE', *, *, #8147, .T. ) ;
#12327 = CARTESIAN_POINT ( 'NONE',  ( -11.93348319268871904, 338.8698905683720000, -2.051577885510841163E-15 ) ) ;
#12328 = CARTESIAN_POINT ( 'NONE',  ( -45.43829269268871229, 343.5573905683720000, -3.332260488124726638 ) ) ;
#12329 = VECTOR ( 'NONE', #3617, 1000.000000000000000 ) ;
#12330 = CARTESIAN_POINT ( 'NONE',  ( -8.685887942688713892, 277.3073905765655809, -3.978247347593165895 ) ) ;
#12331 = PLANE ( 'NONE',  #7574 ) ;
#12332 = CARTESIAN_POINT ( 'NONE',  ( -42.88789093042841927, 252.9323905683720284, -9.489475012073734561 ) ) ;
#12333 = CARTESIAN_POINT ( 'NONE',  ( -42.82802356641967378, 463.2448905765656377, 14.14213562373094923 ) ) ;
#12334 = CARTESIAN_POINT ( 'NONE',  ( -44.16309181155857289, 405.9948905683720568, 6.410867750099241924 ) ) ;
#12335 = EDGE_CURVE ( 'NONE', #2640, #13932, #9015, .T. ) ;
#12336 = VECTOR ( 'NONE', #592, 1000.000000000000000 ) ;
#12337 = DIRECTION ( 'NONE',  ( -0.1337298367054296222, 0.9910178256594273094, -0.000000000000000000 ) ) ;
#12338 = CARTESIAN_POINT ( 'NONE',  ( -40.01497788969913927, 355.6823905601784759, -16.95518130045146421 ) ) ;
#12339 = PRODUCT_DEFINITION_SHAPE ( 'NONE', 'NONE',  #21405 ) ;
#12340 = CARTESIAN_POINT ( 'NONE',  ( -10.20829729246300310, 507.6198905765656377, -7.653668647301794969 ) ) ;
#12341 = CARTESIAN_POINT ( 'NONE',  ( -32.01814843081346140, 471.6823905683720568, -16.75240474999999307 ) ) ;
#12342 = ORIENTED_EDGE ( 'NONE', *, *, #6364, .F. ) ;
#12343 = CARTESIAN_POINT ( 'NONE',  ( -47.16347859291445133, 446.6198905601784759, -7.653668647301793193 ) ) ;
#12344 = AXIS2_PLACEMENT_3D ( 'NONE', #9241, #1044, #10859 ) ;
#12345 = ORIENTED_EDGE ( 'NONE', *, *, #9134, .F. ) ;
#12346 = ORIENTED_EDGE ( 'NONE', *, *, #3113, .F. ) ;
#12347 = VERTEX_POINT ( 'NONE', #92 ) ;
#12348 = CARTESIAN_POINT ( 'NONE',  ( 0.05458999538772797006, -1.264741368073337480, -6.500000000000000888 ) ) ;
#12349 = CARTESIAN_POINT ( 'NONE',  ( -22.27502019258946930, 296.9948905683720000, 15.47720386886985189 ) ) ;
#12350 = EDGE_CURVE ( 'NONE', #3575, #3125, #18339, .T. ) ;
#12351 = AXIS2_PLACEMENT_3D ( 'NONE', #18923, #19042, #17316 ) ;
#12352 = CARTESIAN_POINT ( 'NONE',  ( -11.93348319268872082, 360.3698905683720568, -2.051577885510841163E-15 ) ) ;
#12353 = CARTESIAN_POINT ( 'NONE',  ( -42.82802356641965247, 295.9948905601784759, -14.14213562373094746 ) ) ;
#12354 = CARTESIAN_POINT ( 'NONE',  ( -40.01497788969915348, 513.5573905765656946, 16.95518130045146776 ) ) ;
#12355 = CARTESIAN_POINT ( 'NONE',  ( -35.09675569278795138, 411.9948905683720000, -15.47720386886985544 ) ) ;
#12356 = CARTESIAN_POINT ( 'NONE',  ( -35.09675569278793006, 233.4948905683720284, -15.47720386886985544 ) ) ;
#12357 = CARTESIAN_POINT ( 'NONE',  ( -42.88789093042844058, 412.9323905683720000, -9.489475012073734561 ) ) ;
#12358 =( BOUNDED_CURVE ( )  B_SPLINE_CURVE ( 2, ( #11192, #1159, #15975, #4390, #10974, #6210, #7730, #9668, #6418, #21148, #16294, #20938, #12720, #17583, #19207, #1467, #17688 ),
 .UNSPECIFIED., .F., .T. ) 
 B_SPLINE_CURVE_WITH_KNOTS ( ( 3, 2, 2, 2, 2, 2, 2, 2, 3 ),
 ( 0.4687500000000002220, 0.4707031250000002220, 0.4726562500000002220, 0.4746093750000002220, 0.4765625000000002220, 0.4785156250000002220, 0.4804687500000002220, 0.4824218750000002220, 0.4843750000000002220 ),
 .UNSPECIFIED. ) 
 CURVE ( )  GEOMETRIC_REPRESENTATION_ITEM ( )  RATIONAL_B_SPLINE_CURVE ( ( 0.9999999999999977796, 0.9807852804032326510, 1.000000000000000000, 0.9807852804032304306, 1.000000000000000000, 0.9807852804032304306, 1.000000000000000000, 0.9807852804032304306, 1.000000000000000000, 0.9807852804032304306, 1.000000000000000000, 0.9807852804032304306, 1.000000000000000000, 0.9807852804032304306, 1.000000000000000000, 0.9807852804032282101, 1.000000000000002220 ) ) 
 REPRESENTATION_ITEM ( '' )  );
#12359 = CARTESIAN_POINT ( 'NONE',  ( -8.685887942688719221, 346.6823905765656377, 3.978247347593161010 ) ) ;
#12360 = DIRECTION ( 'NONE',  ( -0.000000000000000000, -1.000000000000000000, -0.000000000000000000 ) ) ;
#12361 = CARTESIAN_POINT ( 'NONE',  ( -22.27502019258946930, 296.9948905683720000, 15.47720386886985189 ) ) ;
#12362 = CARTESIAN_POINT ( 'NONE',  ( -11.93348319268873325, 460.6823905683720568, -3.332260488124732856 ) ) ;
#12363 = EDGE_CURVE ( 'NONE', #313, #11378, #21385, .T. ) ;
#12364 = DIRECTION ( 'NONE',  ( -1.000000000000000000, 0.000000000000000000, 0.000000000000000000 ) ) ;
#12365 = CARTESIAN_POINT ( 'NONE',  ( -28.68588794268874764, 575.7448905601785327, 0.000000000000000000 ) ) ;
#12366 = DIRECTION ( 'NONE',  ( -1.191790137725560488E-16, 1.000000000000000000, -0.000000000000000000 ) ) ;
#12367 = CARTESIAN_POINT ( 'NONE',  ( -45.43829269268870519, 375.0573905683720000, -3.332260488124726194 ) ) ;
#12368 = CARTESIAN_POINT ( 'NONE',  ( -165.7253922195053519, 600.7448905601785327, -108.8355377051282034 ) ) ;
#12369 = CARTESIAN_POINT ( 'NONE',  ( -24.70764059509556887, 510.0573905601785327, 19.99999999999998934 ) ) ;
#12370 = CARTESIAN_POINT ( 'NONE',  ( -14.48388495494899608, 337.9323905683720568, 9.489475012073732785 ) ) ;
#12371 = VERTEX_POINT ( 'NONE', #16526 ) ;
#12372 = CARTESIAN_POINT ( 'NONE',  ( -38.17536295476247687, 512.3073905683719431, -14.20200298773971426 ) ) ;
#12373 = ORIENTED_EDGE ( 'NONE', *, *, #8013, .F. ) ;
#12374 = CARTESIAN_POINT ( 'NONE',  ( -44.08364905673433043, 223.9102039777116602, -6.632192423093624889 ) ) ;
#12375 = DIRECTION ( 'NONE',  ( 0.000000000000000000, 1.000000000000000000, 0.000000000000000000 ) ) ;
#12376 = CARTESIAN_POINT ( 'NONE',  ( -8.685887942688713892, 286.9948905765656377, -2.449293598294705724E-15 ) ) ;
#12377 = CARTESIAN_POINT ( 'NONE',  ( -48.68588794268872988, 521.9948905765656946, 0.000000000000000000 ) ) ;
#12378 = CARTESIAN_POINT ( 'NONE',  ( -22.27502019258949773, 470.7448905683720568, -15.47720386886985544 ) ) ;
#12379 = ORIENTED_EDGE ( 'NONE', *, *, #12393, .T. ) ;
#12380 = CARTESIAN_POINT ( 'NONE',  ( -35.09675569278795848, 471.9948905683720000, -15.47720386886985544 ) ) ;
#12381 = CARTESIAN_POINT ( 'NONE',  ( -17.35679799567827786, 250.6823905601785043, 16.95518130045146421 ) ) ;
#12382 = CARTESIAN_POINT ( 'NONE',  ( -42.82802356641966668, 403.2448905765655809, 14.14213562373094923 ) ) ;
#12383 = CARTESIAN_POINT ( 'NONE',  ( 0.000000000000000000, 610.7448905601785327, 0.000000000000000000 ) ) ;
#12384 = CARTESIAN_POINT ( 'NONE',  ( -17.35679799567828141, 300.6823905601784759, 16.95518130045146421 ) ) ;
#12385 = DIRECTION ( 'NONE',  ( -1.191790137725560488E-16, 1.000000000000000000, -0.000000000000000000 ) ) ;
#12386 = DIRECTION ( 'NONE',  ( -1.191790137725560488E-16, 1.000000000000000000, -0.000000000000000000 ) ) ;
#12387 = DIRECTION ( 'NONE',  ( 1.000000000000000000, 0.000000000000000000, 0.000000000000000000 ) ) ;
#12388 = CARTESIAN_POINT ( 'NONE',  ( -40.01497788969911795, 238.8073905601784759, 16.95518130045146776 ) ) ;
#12389 = CARTESIAN_POINT ( 'NONE',  ( 0.01372220897661874210, -5.309964801958117597, 3.802871176606137826 ) ) ;
#12390 = EDGE_CURVE ( 'NONE', #16401, #16623, #6551, .T. ) ;
#12391 = CARTESIAN_POINT ( 'NONE',  ( -11.93348319268871016, 280.3698905683720000, -2.051577885510841163E-15 ) ) ;
#12392 = AXIS2_PLACEMENT_3D ( 'NONE', #639, #17808, #17392 ) ;
#12393 = EDGE_CURVE ( 'NONE', #9678, #20528, #1293, .T. ) ;
#12394 = CARTESIAN_POINT ( 'NONE',  ( -36.33955658999049376, 255.3698905601785043, -18.47759065022572855 ) ) ;
#12395 = CARTESIAN_POINT ( 'NONE',  ( 35.96497763894178945, 230.5765313837437418, -60.00000000000000000 ) ) ;
#12396 = CARTESIAN_POINT ( 'NONE',  ( -25.35362745456398770, 428.1823905683720000, 16.75240474999998952 ) ) ;
#12397 = CARTESIAN_POINT ( 'NONE',  ( -17.35679799567829207, 328.5573905765656377, -16.95518130045146421 ) ) ;
#12398 = CARTESIAN_POINT ( 'NONE',  ( -13.20868407381884957, 270.9948905683720000, -6.410867750099233042 ) ) ;
#12399 = VERTEX_POINT ( 'NONE', #3954 ) ;
#12400 = CARTESIAN_POINT ( 'NONE',  ( -18.68588794268873698, 281.1055109169419666, 40.00000000000000000 ) ) ;
#12401 = PRODUCT_RELATED_PRODUCT_CATEGORY ( 'part', '', ( #19604 ) ) ;
#12402 = ORIENTED_EDGE ( 'NONE', *, *, #6564, .F. ) ;
#12403 = CARTESIAN_POINT ( 'NONE',  ( -35.09675569278796559, 487.2448905683720000, 15.47720386886985366 ) ) ;
#12404 = ORIENTED_EDGE ( 'NONE', *, *, #2611, .F. ) ;
#12405 = CARTESIAN_POINT ( 'NONE',  ( -5.502341142637719784, 585.7448905601785327, -7.573322868991255952 ) ) ;
#12406 = CARTESIAN_POINT ( 'NONE',  ( -42.88789093042841927, 234.8073905683720284, 9.489475012073736337 ) ) ;
#12407 = ORIENTED_EDGE ( 'NONE', *, *, #5647, .T. ) ;
#12408 = CARTESIAN_POINT ( 'NONE',  ( 158.8141120573112630, 400.5398297725602674, -5.000000000000004441 ) ) ;
#12409 = AXIS2_PLACEMENT_3D ( 'NONE', #11826, #10088, #15511 ) ;
#12410 = CARTESIAN_POINT ( 'NONE',  ( -36.33955658999052218, 470.1198905765656377, -18.47759065022572855 ) ) ;
#12411 = LINE ( 'NONE', #20742, #5817 ) ;
#12412 = CARTESIAN_POINT ( 'NONE',  ( 170.2047888904039610, 610.7448905601785327, -1.893624729818132124 ) ) ;
#12413 = CARTESIAN_POINT ( 'NONE',  ( -36.33955658999052218, 455.3698905601784759, -18.47759065022572855 ) ) ;
#12414 = CARTESIAN_POINT ( 'NONE',  ( -38.17536295476243424, 226.9323905683720000, 14.20200298773971781 ) ) ;
#12415 = CARTESIAN_POINT ( 'NONE',  ( -44.16309181155859420, 524.7448905683720568, -6.410867750099231266 ) ) ;
#12416 = CARTESIAN_POINT ( 'NONE',  ( 6.416697501590670427, 217.7548513357008630, 45.00000000000000000 ) ) ;
#12417 = VECTOR ( 'NONE', #13799, 1000.000000000000000 ) ;
#12418 = CARTESIAN_POINT ( 'NONE',  ( -22.27502019258947286, 240.7448905683720000, -15.47720386886985544 ) ) ;
#12419 = CARTESIAN_POINT ( 'NONE',  ( -42.88789093042843348, 336.3073905683720568, 9.489475012073736337 ) ) ;
#12420 = CARTESIAN_POINT ( 'NONE',  ( -42.82802356641967378, 468.4948905601785327, 14.14213562373094923 ) ) ;
#12421 = CARTESIAN_POINT ( 'NONE',  ( -28.68588794268871212, 359.7448905601784759, 19.99999999999999289 ) ) ;
#12422 = VECTOR ( 'NONE', #6282, 1000.000000000000000 ) ;
#12423 = CARTESIAN_POINT ( 'NONE',  ( -35.09675569278795138, 385.7448905683720000, 15.47720386886985366 ) ) ;
#12424 = FACE_OUTER_BOUND ( 'NONE', #11202, .T. ) ;
#12425 = CARTESIAN_POINT ( 'NONE',  ( -8.685887942688724550, 382.2448905601784759, -2.449293598294705724E-15 ) ) ;
#12426 = VECTOR ( 'NONE', #8365, 1000.000000000000000 ) ;
#12427 = ORIENTED_EDGE ( 'NONE', *, *, #11871, .T. ) ;
#12428 = CARTESIAN_POINT ( 'NONE',  ( -48.68588794268858067, 406.9323905601785327, -3.978247347593477201 ) ) ;
#12429 = ORIENTED_EDGE ( 'NONE', *, *, #7481, .T. ) ;
#12430 = VERTEX_POINT ( 'NONE', #14030 ) ;
#12431 = CARTESIAN_POINT ( 'NONE',  ( -16.84014894278200813, 501.6198905683720000, -11.84573899990672707 ) ) ;
#12432 = CARTESIAN_POINT ( 'NONE',  ( -28.68588794268874054, 573.2448905601785327, 0.000000000000000000 ) ) ;
#12433 = ORIENTED_EDGE ( 'NONE', *, *, #3102, .F. ) ;
#12434 = CARTESIAN_POINT ( 'NONE',  ( -38.17536295476244135, 296.9323905683720000, 14.20200298773971781 ) ) ;
#12435 = ORIENTED_EDGE ( 'NONE', *, *, #11201, .F. ) ;
#12436 = CARTESIAN_POINT ( 'NONE',  ( -13.20868407381885845, 339.4948905683720568, -6.410867750099233042 ) ) ;
#12437 = CARTESIAN_POINT ( 'NONE',  ( -22.27502019258947286, 336.9948905683720000, 15.47720386886985189 ) ) ;
#12438 = CARTESIAN_POINT ( 'NONE',  ( -48.68588794268870146, 281.9948905765656377, 0.000000000000000000 ) ) ;
#12439 = CARTESIAN_POINT ( 'NONE',  ( -28.68588794268871922, 394.7448905601784759, -19.99999999999999289 ) ) ;
#12440 = CARTESIAN_POINT ( 'NONE',  ( -16.84014894278197616, 250.1198905683720284, -11.84573899990672707 ) ) ;
#12441 = DIRECTION ( 'NONE',  ( -1.191790137725560488E-16, 1.000000000000000000, -0.000000000000000000 ) ) ;
#12442 = CARTESIAN_POINT ( 'NONE',  ( -16.84014894278199037, 389.1198905683720568, 11.84573899990672530 ) ) ;
#12443 = CARTESIAN_POINT ( 'NONE',  ( -8.685887942688719221, 332.2448905601784759, -2.449293598294705724E-15 ) ) ;
#12444 = DIRECTION ( 'NONE',  ( -1.191790137725560488E-16, 1.000000000000000000, 0.000000000000000000 ) ) ;
#12445 = CLOSED_SHELL ( 'NONE', ( #9805, #12549, #9483, #19623, #787, #10980, #1369, #20963, #18337, #9873, #2888, #2174, #701, #11465, #11452, #4014, #11112, #20791, #4988, #437, #316, #19924, #7975, #16891, #11273, #10078, #16197, #6526, #7541, #3486, #3547, #6617, #11026, #11397, #21189, #5793, #20199, #15343, #15715, #11059, #15405, #16633, #7757, #11914, #17026, #15059, #13333, #13418, #12087, #13190, #14189, #11777, #10668, #4380, #12976, #3293, #3760, #17294, #19076, #19982, #12149, #12215, #2349, #13536, #19105, #919, #7617, #19155, #17850, #8883, #2956, #3979, #7767, #12261, #2618, #1058, #19340, #384, #8936 ) ) ;
#12446 = LINE ( 'NONE', #9932, #1155 ) ;
#12447 = CARTESIAN_POINT ( 'NONE',  ( -35.09675569278795848, 445.7448905683720000, 15.47720386886985366 ) ) ;
#12448 = ORIENTED_EDGE ( 'NONE', *, *, #13913, .F. ) ;
#12449 = CARTESIAN_POINT ( 'NONE',  ( -14.54375231895778064, 453.4948905601784759, -14.14213562373094746 ) ) ;
#12450 = VERTEX_POINT ( 'NONE', #15337 ) ;
#12451 =( GEOMETRIC_REPRESENTATION_CONTEXT ( 3 ) GLOBAL_UNCERTAINTY_ASSIGNED_CONTEXT ( ( #18926 ) ) GLOBAL_UNIT_ASSIGNED_CONTEXT ( ( #12998, #9636, #3869 ) ) REPRESENTATION_CONTEXT ( 'NONE', 'WORKASPACE' ) );
#12452 = ORIENTED_EDGE ( 'NONE', *, *, #16038, .T. ) ;
#12453 = ORIENTED_EDGE ( 'NONE', *, *, #20470, .F. ) ;
#12454 = FACE_OUTER_BOUND ( 'NONE', #17478, .T. ) ;
#12455 = CARTESIAN_POINT ( 'NONE',  ( -47.16347859291443712, 326.6198905601784759, -7.653668647301793193 ) ) ;
#12456 = CARTESIAN_POINT ( 'NONE',  ( -44.16309181155856578, 303.2448905683720000, -6.410867750099231266 ) ) ;
#12457 = EDGE_CURVE ( 'NONE', #11839, #15497, #6982, .T. ) ;
#12458 = CARTESIAN_POINT ( 'NONE',  ( -11.93348319268872260, 360.6823905683720568, -3.332260488124732856 ) ) ;
#12459=STYLED_ITEM('',(#21442),#11980);
#12460 = CARTESIAN_POINT ( 'NONE',  ( -8.685887942688713892, 292.2448905601784759, -2.449293598294705724E-15 ) ) ;
#12461 = CIRCLE ( 'NONE', #9686, 50.00000000000000000 ) ;
#12462 = CARTESIAN_POINT ( 'NONE',  ( -45.64106924314020119, 522.9323905765656946, 11.32908994701042715 ) ) ;
#12463 = CARTESIAN_POINT ( 'NONE',  ( -38.17536295476246266, 402.3073905683720000, -14.20200298773971426 ) ) ;
#12464 = CARTESIAN_POINT ( 'NONE',  ( -13.20868407381884779, 240.9948905683720284, -6.410867750099233042 ) ) ;
#12465 = CIRCLE ( 'NONE', #8651, 175.0000000000000284 ) ;
#12466 = CARTESIAN_POINT ( 'NONE',  ( -25.35362745456399480, 401.0573905683720568, -16.75240474999999307 ) ) ;
#12467 = CONTEXT_DEPENDENT_SHAPE_REPRESENTATION ( #4467, #13050 ) ;
#12468 = CARTESIAN_POINT ( 'NONE',  ( -21.03221929538691981, 338.8698905765656377, -18.47759065022572855 ) ) ;
#12469 = FACE_OUTER_BOUND ( 'NONE', #15136, .T. ) ;
#12470 = CARTESIAN_POINT ( 'NONE',  ( -35.09675569278794427, 315.7448905683720000, 15.47720386886985366 ) ) ;
#12471 = VECTOR ( 'NONE', #8159, 1000.000000000000000 ) ;
#12472 = CARTESIAN_POINT ( 'NONE',  ( -45.43829269268872650, 455.3698905683720000, 0.000000000000000000 ) ) ;
#12474 = CARTESIAN_POINT ( 'NONE',  ( -48.68588794268887909, 457.5573905601783622, 3.978247347592742678 ) ) ;
#12473 = AXIS2_PLACEMENT_3D ( 'NONE', #21241, #21134, #6307 ) ;
#12475 = CYLINDRICAL_SURFACE ( 'NONE', #2125, 19.99999999999999645 ) ;
#12476 = CARTESIAN_POINT ( 'NONE',  ( 5.074999999999999289, 5.629165124598848990, 3.250000000000006217 ) ) ;
#12477 = ADVANCED_FACE ( 'NONE', ( #727 ), #11959, .T. ) ;
#12478 = CIRCLE ( 'NONE', #1424, 175.0000000000000284 ) ;
#12479 = CARTESIAN_POINT ( 'NONE',  ( -42.88789093042843348, 374.4323905683720000, -9.489475012073736337 ) ) ;
#12480 = CONICAL_SURFACE ( 'NONE', #16979, 6.500000000000000000, 1.047197551196600296 ) ;
#12481 = CARTESIAN_POINT ( 'NONE',  ( -19.19641293061499709, 497.3073905683720568, 14.20200298773971426 ) ) ;
#12482 = CARTESIAN_POINT ( 'NONE',  ( -14.54375231895778420, 500.9948905601784190, 14.14213562373094568 ) ) ;
#12483 = CARTESIAN_POINT ( 'NONE',  ( -13.20868407381885845, 349.4948905683720000, -6.410867750099233042 ) ) ;
#12484 = ORIENTED_EDGE ( 'NONE', *, *, #12533, .F. ) ;
#12485 = CARTESIAN_POINT ( 'NONE',  ( -11.93348319268873858, 499.1823905683720568, -3.332260488124732856 ) ) ;
#12486 = ORIENTED_EDGE ( 'NONE', *, *, #13664, .T. ) ;
#12487 = AXIS2_PLACEMENT_3D ( 'NONE', #16863, #18673, #3862 ) ;
#12488 =( BOUNDED_CURVE ( )  B_SPLINE_CURVE ( 2, ( #8665, #9855, #16483, #3490, #11813, #15289, #3596, #10179, #474, #1989, #14967, #6936, #1665, #7040, #5107, #15078, #263 ),
 .UNSPECIFIED., .F., .T. ) 
 B_SPLINE_CURVE_WITH_KNOTS ( ( 3, 2, 2, 2, 2, 2, 2, 2, 3 ),
 ( 0.5781250000000001110, 0.5800781250000001110, 0.5820312500000001110, 0.5839843750000001110, 0.5859375000000002220, 0.5878906250000002220, 0.5898437500000002220, 0.5917968750000002220, 0.5937500000000002220 ),
 .UNSPECIFIED. ) 
 CURVE ( )  GEOMETRIC_REPRESENTATION_ITEM ( )  RATIONAL_B_SPLINE_CURVE ( ( 0.9999999999999988898, 0.9807852804032315408, 1.000000000000000000, 0.9807852804032304306, 1.000000000000000000, 0.9807852804032304306, 1.000000000000000000, 0.9807852804032304306, 1.000000000000000000, 0.9807852804032304306, 1.000000000000000000, 0.9807852804032304306, 1.000000000000000000, 0.9807852804032304306, 1.000000000000000000, 0.9807852804032282101, 1.000000000000002220 ) ) 
 REPRESENTATION_ITEM ( '' )  );
#12489 = CARTESIAN_POINT ( 'NONE',  ( -43.68588794268873698, 573.2448905601785327, 0.000000000000000000 ) ) ;
#12490 = EDGE_CURVE ( 'NONE', #8423, #15264, #19728, .T. ) ;
#12491 = CARTESIAN_POINT ( 'NONE',  ( -38.17536295476246266, 433.8073905683721136, -14.20200298773971426 ) ) ;
#12492 = LINE ( 'NONE', #2538, #13494 ) ;
#12493 = CARTESIAN_POINT ( 'NONE',  ( 27.98965548446208729, 333.8848358243226357, 40.00000000000000000 ) ) ;
#12494 = CARTESIAN_POINT ( 'NONE',  ( -45.43829269268872650, 463.8698905683720000, 0.000000000000000000 ) ) ;
#12495 = EDGE_LOOP ( 'NONE', ( #10528, #17116, #8509, #9070, #216 ) ) ;
#12496 = CARTESIAN_POINT ( 'NONE',  ( -42.88789093042844769, 474.8073905683720000, 9.489475012073734561 ) ) ;
#12497 = DIRECTION ( 'NONE',  ( -1.191790137725560488E-16, 1.000000000000000000, -0.000000000000000000 ) ) ;
#12498 = CARTESIAN_POINT ( 'NONE',  ( -36.33955658999051508, 400.1198905765656377, -18.47759065022572855 ) ) ;
#12499 = CARTESIAN_POINT ( 'NONE',  ( -18.68588794268873698, 323.8848358243226357, -40.00000000000000000 ) ) ;
#12500 = DIRECTION ( 'NONE',  ( -1.000000000000000000, 0.000000000000000000, 0.000000000000000000 ) ) ;
#12501 = DIRECTION ( 'NONE',  ( -9.855701800883827197E-17, 1.000000000000000000, -0.000000000000000000 ) ) ;
#12502 = CARTESIAN_POINT ( 'NONE',  ( 10.41669750159067220, 217.7548513357008630, 49.99999999999999289 ) ) ;
#12503 = CARTESIAN_POINT ( 'NONE',  ( -33.84809828339280102, 56.85652257517428865, 120.3299889578561448 ) ) ;
#12504 = DIRECTION ( 'NONE',  ( 1.000000000000000000, 0.000000000000000000, 0.000000000000000000 ) ) ;
#12505 = DIRECTION ( 'NONE',  ( 0.000000000000000000, 1.000000000000000000, -0.000000000000000000 ) ) ;
#12506 = CARTESIAN_POINT ( 'NONE',  ( -44.16309181155856578, 274.7448905683720568, -6.410867750099231266 ) ) ;
#12507 = CARTESIAN_POINT ( 'NONE',  ( -14.54375231895775222, 250.9948905601784759, 14.14213562373094568 ) ) ;
#12508 = DIRECTION ( 'NONE',  ( 0.000000000000000000, 1.000000000000000000, 0.000000000000000000 ) ) ;
#12509 = CARTESIAN_POINT ( 'NONE',  ( -32.01814843081345430, 423.1823905683720568, -16.75240474999999307 ) ) ;
#12510 = CARTESIAN_POINT ( 'NONE',  ( 162.8695233526006803, 620.7448905601785327, -10.81142786866620575 ) ) ;
#12511 = CARTESIAN_POINT ( 'NONE',  ( -38.17536295476244135, 253.8073905683720568, -14.20200298773971426 ) ) ;
#12512 = ORIENTED_EDGE ( 'NONE', *, *, #9621, .F. ) ;
#12513 = ORIENTED_EDGE ( 'NONE', *, *, #10616, .T. ) ;
#12514 = ORIENTED_EDGE ( 'NONE', *, *, #16643, .F. ) ;
#12515 = CARTESIAN_POINT ( 'NONE',  ( -35.09675569278796559, 477.2448905683720568, 15.47720386886985366 ) ) ;
#12516 =( GEOMETRIC_REPRESENTATION_CONTEXT ( 3 ) GLOBAL_UNCERTAINTY_ASSIGNED_CONTEXT ( ( #12210 ) ) GLOBAL_UNIT_ASSIGNED_CONTEXT ( ( #16096, #8064, #4516 ) ) REPRESENTATION_CONTEXT ( 'NONE', 'WORKASPACE' ) );
#12517 = ORIENTED_EDGE ( 'NONE', *, *, #13055, .F. ) ;
#12518 = CARTESIAN_POINT ( 'NONE',  ( -45.64106924314017988, 366.3073905601785896, -11.32908994701042538 ) ) ;
#12519 = CARTESIAN_POINT ( 'NONE',  ( -45.43829269268869098, 234.1823905683720284, 3.332260488124734632 ) ) ;
#12520 = VERTEX_POINT ( 'NONE', #2449 ) ;
#12521 = DIRECTION ( 'NONE',  ( -1.000000000000000000, 0.000000000000000000, 0.000000000000000000 ) ) ;
#12522 = CARTESIAN_POINT ( 'NONE',  ( 115.7989814974898337, 142.5259582928263455, -20.00000000000000355 ) ) ;
#12523 = CARTESIAN_POINT ( 'NONE',  ( -32.66413529028189089, 459.8073905765656377, -19.99999999999999289 ) ) ;
#12524 = CARTESIAN_POINT ( 'NONE',  ( -11.73070664223724613, 351.3073905601785327, 11.32908994701042005 ) ) ;
#12525 = CARTESIAN_POINT ( 'NONE',  ( -47.16347859291443712, 282.6198905765656377, 7.653668647301805628 ) ) ;
#12526 = CARTESIAN_POINT ( 'NONE',  ( -11.73070664223726034, 453.1823905601785327, -11.32908994701042538 ) ) ;
#12527 = DIRECTION ( 'NONE',  ( 0.000000000000000000, 0.000000000000000000, -1.000000000000000000 ) ) ;
#12528 = CARTESIAN_POINT ( 'NONE',  ( -40.53162694259545873, 524.1198905683720568, -11.84573899990672707 ) ) ;
#12529 = CARTESIAN_POINT ( 'NONE',  ( -24.70764059509555111, 374.8073905765655809, 19.99999999999998934 ) ) ;
#12530 = CARTESIAN_POINT ( 'NONE',  ( -38.17536295476244135, 252.3073905683720284, -14.20200298773971426 ) ) ;
#12531 = CIRCLE ( 'NONE', #16676, 15.00000000000000355 ) ;
#12532 = CARTESIAN_POINT ( 'NONE',  ( -22.27502019258948351, 342.2448905683720568, -15.47720386886985544 ) ) ;
#12533 = EDGE_CURVE ( 'NONE', #5288, #1858, #20610, .T. ) ;
#12534 = CARTESIAN_POINT ( 'NONE',  ( 0.000000000000000000, 0.000000000000000000, 0.000000000000000000 ) ) ;
#12535 = CARTESIAN_POINT ( 'NONE',  ( -40.01497788969912506, 273.5573905765656377, 16.95518130045146776 ) ) ;
#12536 = EDGE_CURVE ( 'NONE', #20892, #795, #14557, .T. ) ;
#12537 = ADVANCED_FACE ( 'NONE', ( #7297 ), #5680, .F. ) ;
#12538 = CARTESIAN_POINT ( 'NONE',  ( -13.20868407381886200, 379.4948905683720000, -6.410867750099233042 ) ) ;
#12539 = DIRECTION ( 'NONE',  ( -1.000000000000000000, -0.000000000000000000, -0.000000000000000000 ) ) ;
#12540 = AXIS2_PLACEMENT_3D ( 'NONE', #835, #7401, #14555 ) ;
#12541 = CARTESIAN_POINT ( 'NONE',  ( -40.01497788969913927, 385.6823905601784190, -16.95518130045146421 ) ) ;
#12542 = VERTEX_POINT ( 'NONE', #15653 ) ;
#12543 = CARTESIAN_POINT ( 'NONE',  ( -11.73070664223725501, 403.1823905601785896, -11.32908994701042538 ) ) ;
#12544 = ORIENTED_EDGE ( 'NONE', *, *, #12457, .F. ) ;
#12545 = ORIENTED_EDGE ( 'NONE', *, *, #17936, .F. ) ;
#12546 = CARTESIAN_POINT ( 'NONE',  ( -45.43829269268873361, 515.3698905683720568, 0.000000000000000000 ) ) ;
#12547 = DIRECTION ( 'NONE',  ( -0.000000000000000000, -1.000000000000000000, -0.000000000000000000 ) ) ;
#12548 = ORIENTED_EDGE ( 'NONE', *, *, #7052, .T. ) ;
#12549 = ADVANCED_FACE ( 'NONE', ( #5786 ), #12287, .T. ) ;
#12550 = CARTESIAN_POINT ( 'NONE',  ( -32.01814843081344009, 297.5573905683720000, 16.75240474999999307 ) ) ;
#12551 = ORIENTED_EDGE ( 'NONE', *, *, #13411, .F. ) ;
#12552 = CARTESIAN_POINT ( 'NONE',  ( -13.20868407381885312, 318.2448905683720000, 6.410867750099229490 ) ) ;
#12553 = CARTESIAN_POINT ( 'NONE',  ( -19.19641293061498288, 350.4323905683720000, -14.20200298773971603 ) ) ;
#12554 = AXIS2_PLACEMENT_3D ( 'NONE', #8235, #10284, #9968 ) ;
#12555 = CARTESIAN_POINT ( 'NONE',  ( -32.66413529028186957, 274.1823905765656377, 19.99999999999999289 ) ) ;
#12556 = CARTESIAN_POINT ( 'NONE',  ( -17.35679799567829917, 393.8073905601785327, -16.95518130045146421 ) ) ;
#12557 = CARTESIAN_POINT ( 'NONE',  ( -32.01814843081343298, 246.0573905683720000, 16.75240474999999307 ) ) ;
#12558 = CARTESIAN_POINT ( 'NONE',  ( -36.33955658999049376, 225.3698905601784759, -18.47759065022572855 ) ) ;
#12559 = AXIS2_PLACEMENT_3D ( 'NONE', #9689, #3427, #19863 ) ;
#12560 = CARTESIAN_POINT ( 'NONE',  ( -42.88789093042844058, 394.4323905683720000, -9.489475012073736337 ) ) ;
#12561 = DIRECTION ( 'NONE',  ( 0.000000000000000000, 0.000000000000000000, 1.000000000000000000 ) ) ;
#12562 = LINE ( 'NONE', #4436, #11077 ) ;
#12563 = DIRECTION ( 'NONE',  ( 0.000000000000000000, -1.000000000000000000, 0.000000000000000000 ) ) ;
#12564 = CARTESIAN_POINT ( 'NONE',  ( -32.01814843081345430, 441.6823905683721136, -16.75240474999999307 ) ) ;
#12565 = ORIENTED_EDGE ( 'NONE', *, *, #1574, .F. ) ;
#12566 = CARTESIAN_POINT ( 'NONE',  ( -10.20829729246299600, 452.8698905601785327, -7.653668647301794969 ) ) ;
#12567 = VECTOR ( 'NONE', #1005, 1000.000000000000000 ) ;
#12568 = ORIENTED_EDGE ( 'NONE', *, *, #8275, .T. ) ;
#12569 = EDGE_LOOP ( 'NONE', ( #10921, #5582, #8204, #14064 ) ) ;
#12570 = FACE_OUTER_BOUND ( 'NONE', #19856, .T. ) ;
#12571 = CARTESIAN_POINT ( 'NONE',  ( -8.685887942688717445, 332.5573905601784190, -3.978247347593165895 ) ) ;
#12572 = VECTOR ( 'NONE', #12501, 1000.000000000000000 ) ;
#12573 = CARTESIAN_POINT ( 'NONE',  ( -16.84014894278198682, 359.1198905683720568, 11.84573899990672530 ) ) ;
#12574 = FACE_OUTER_BOUND ( 'NONE', #10028, .T. ) ;
#12575 = CARTESIAN_POINT ( 'NONE',  ( -48.68588794268872277, 502.3073905765656946, 3.978247347593168115 ) ) ;
#12576 = CARTESIAN_POINT ( 'NONE',  ( -40.53162694259543741, 385.1198905683720568, 11.84573899990672885 ) ) ;
#12577 = CARTESIAN_POINT ( 'NONE',  ( -22.27502019258946220, 238.4948905683720284, 15.47720386886985189 ) ) ;
#12578 = CARTESIAN_POINT ( 'NONE',  ( -14.48388495494900674, 409.8073905683720568, -9.489475012073734561 ) ) ;
#12579 = CARTESIAN_POINT ( 'NONE',  ( -17.35679799567829917, 348.5573905765655809, -16.95518130045146421 ) ) ;
#12580 = CARTESIAN_POINT ( 'NONE',  ( -32.66413529028186247, 325.0573905601785327, -19.99999999999999289 ) ) ;
#12581 = CARTESIAN_POINT ( 'NONE',  ( -14.48388495494899075, 307.9323905683719431, 9.489475012073731008 ) ) ;
#12582 = CARTESIAN_POINT ( 'NONE',  ( -42.88789093042844769, 454.4323905683720568, -9.489475012073736337 ) ) ;
#12583 = FACE_OUTER_BOUND ( 'NONE', #6041, .T. ) ;
#12584 = DIRECTION ( 'NONE',  ( 0.6352526299242177155, 0.000000000000000000, 0.7723044064191041391 ) ) ;
#12585 = DIRECTION ( 'NONE',  ( -0.000000000000000000, -1.000000000000000000, -0.000000000000000000 ) ) ;
#12586 = AXIS2_PLACEMENT_3D ( 'NONE', #15258, #20217, #5074 ) ;
#12587 = ADVANCED_FACE ( 'NONE', ( #3848 ), #4060, .T. ) ;
#12588 = CARTESIAN_POINT ( 'NONE',  ( -13.20868407381886023, 360.9948905683720568, -6.410867750099233042 ) ) ;
#12589 = CARTESIAN_POINT ( 'NONE',  ( -22.27502019258949417, 496.9948905683720568, 15.47720386886985189 ) ) ;
#12590 = CARTESIAN_POINT ( 'NONE',  ( -42.82802356641967378, 498.4948905601784759, 14.14213562373094923 ) ) ;
#12591 = CARTESIAN_POINT ( 'NONE',  ( -19.19641293061498288, 320.4323905683720568, -14.20200298773971603 ) ) ;
#12592 = ORIENTED_EDGE ( 'NONE', *, *, #19135, .F. ) ;
#12593 = CARTESIAN_POINT ( 'NONE',  ( -14.48388495494901740, 499.8073905683720568, -9.489475012073736337 ) ) ;
#12594 = EDGE_LOOP ( 'NONE', ( #18485, #18644, #16726, #20352 ) ) ;
#12595 = EDGE_CURVE ( 'NONE', #9304, #11578, #6241, .T. ) ;
#12596 = CARTESIAN_POINT ( 'NONE',  ( -36.33955658999050797, 313.8698905765656377, 18.47759065022572500 ) ) ;
#12597 = CARTESIAN_POINT ( 'NONE',  ( -32.01814843081344719, 433.1823905683720568, -16.75240474999999307 ) ) ;
#12598 = CARTESIAN_POINT ( 'NONE',  ( -42.82802356641966668, 393.2448905765655809, 14.14213562373094923 ) ) ;
#12599 = SURFACE_STYLE_FILL_AREA ( #5989 ) ;
#12600 = CARTESIAN_POINT ( 'NONE',  ( -35.09675569278795848, 461.9948905683720000, -15.47720386886985544 ) ) ;
#12601 = ORIENTED_EDGE ( 'NONE', *, *, #6130, .F. ) ;
#12602 = CARTESIAN_POINT ( 'NONE',  ( -38.17536295476246266, 475.4323905683720000, 14.20200298773971781 ) ) ;
#12603 = CARTESIAN_POINT ( 'NONE',  ( -8.685887942688884422, 246.6823905765655809, 3.978247347593586447 ) ) ;
#12604 = CARTESIAN_POINT ( 'NONE',  ( -40.01497788969914637, 400.4323905765656377, -16.95518130045146421 ) ) ;
#12605 = CARTESIAN_POINT ( 'NONE',  ( 21.30000000000000071, 4.475777889183788807E-16, -3.309499999999999886 ) ) ;
#12606 = EDGE_CURVE ( 'NONE', #17381, #952, #15756, .T. ) ;
#12607 = CARTESIAN_POINT ( 'NONE',  ( -48.68588794268870856, 387.2448905601784759, 0.000000000000000000 ) ) ;
#12608 = FACE_OUTER_BOUND ( 'NONE', #8157, .T. ) ;
#12609 = CARTESIAN_POINT ( 'NONE',  ( 18.55315245287936321, 130.1716627696692683, -25.00000000000000000 ) ) ;
#12610 = CARTESIAN_POINT ( 'NONE',  ( 105.7989814974898479, 142.5259582928263455, -40.00000000000000000 ) ) ;
#12611 = CARTESIAN_POINT ( 'NONE',  ( -45.55770059569361763, 223.9102039777116886, 1.340232597368489209 ) ) ;
#12612 = EDGE_CURVE ( 'NONE', #15843, #19525, #12900, .T. ) ;
#12613 = CARTESIAN_POINT ( 'NONE',  ( -48.68588794268869435, 257.5573905601784759, 3.978247347593168115 ) ) ;
#12614 = CARTESIAN_POINT ( 'NONE',  ( -24.70764059509555821, 450.0573905601785327, 19.99999999999998934 ) ) ;
#12615 = CARTESIAN_POINT ( 'NONE',  ( -38.17536295476245556, 426.9323905683720000, 14.20200298773971781 ) ) ;
#12616 = FACE_OUTER_BOUND ( 'NONE', #20564, .T. ) ;
#12617 =( BOUNDED_SURFACE ( )  B_SPLINE_SURFACE ( 1, 2, ( 
 ( #10827, #12250, #12027, #4126, #20360, #5743, #20680, #14099, #18726, #7150, #4018, #13771, #7469, #2515, #582, #5642, #18941, #12140, #15399, #904, #10714, #7366, #5535, #17332, #3806, #7578, #18833, #15720, #15828, #12462, #10397, #19060, #3914, #2621, #10611, #1012, #2198, #17437, #10504, #7257, #17125, #17016, #2304, #8887, #9202, #689, #15504, #17229, #8783, #14205, #800, #15613, #20794, #13882, #20473, #2412, #8992, #13993, #20575, #12354, #1219, #4450, #20897, #21215, #1426, #6277, #19375, #4347, #16247, #2839, #14630, #9733, #2943, #11036, #6380, #9628, #14732, #12989, #5961, #14422, #12676, #19582, #16355, #9421, #15928, #17647, #1532, #9522, #3154, #8102, #16140, #21105, #12891, #6171, #4560, #12575, #19270, #19169, #7998, #10930, #7892, #16041, #1117, #4762, #19481, #1321, #6065, #4661, #17540, #2731, #12781, #11252, #9311, #17851, #7688, #3045, #7789, #17954, #11147, #14318, #21003, #11357, #17752, #14520, #16459, #4873, #14842, #18, #13826, #9947, #6594, #14947, #13102, #10558, #10346, #3467, #5485, #1642, #13215, #638, #19800, #4980, #8325, #9836, #16567, #11579, #18170, #15454, #17074, #536, #13323, #19687, #10454, #3368, #8834, #3968, #18279, #1753, #7204, #3864, #8940, #20419, #21314, #133, #6706, #5593, #17181, #19906, #8214, #5087, #2360, #16969, #18784, #6485, #2149, #15355, #7102, #11688, #8730, #11467, #13723, #18065, #2256, #3260, #20313, #12083, #18676, #12196, #13942, #17391, #5803, #20629, #10664, #7744, #17282, #15775, #14264, #15882, #12410, #19002, #9047, #15670, #17490, #4188, #14373, #4511, #19222, #20954, #10774, #2573, #856, #2467, #6124, #964, #15563, #7640, #7420, #9264, #2788, #17597, #14046, #9153, #7528, #14154, #10987, #6021, #4078, #20741, #1070, #5913, #18892, #12523, #20530, #4406, #19117, #9375, #19324, #4300, #2679, #15992, #1172, #2899, #12733, #748, #20851, #12631, #11099, #17702, #7313, #5695, #12302, #13275, #6436, #6653, #19860, #19638, #3211, #9789, #9685, #8058, #5036, #1376, #11638, #13161, #1269, #11414, #6336, #4615, #7848, #14475, #11311, #21162, #14578, #11210, #1702, #17807, #16309, #8161, #16412, #12948, #19537, #2998, #9582, #4819, #4714, #8270, #18232, #19749, #14901, #17906, #3103, #16198, #7948, #86, #1481, #9479, #1590, #14689, #14794, #18122, #11531, #21266, #13049, #18017, #21375, #4932, #6544, #19430, #3317, #9897, #16519, #12841, #16090, #21058, #6227, #18340, #10319, #10004, #20391, #3633, #8705, #7178, #16942, #16627, #15329, #3527, #15428, #16839, #13801, #15010, #7074, #16737, #20080, #19969, #8384, #10115, #1924, #17050, #13486, #8491, #18448, #1817, #5567, #13596, #6974, #513, #5148, #15116, #3839, #298, #6867, #11851, #13380, #5252, #10216, #2027, #18648, #20288, #3733, #8594, #15217, #12172, #409, #8811, #20183, #5351, #10428, #11952, #13695, #2124, #18548, #5458, #12059, #2232, #614, #3424, #194, #6762, #11746, #17462, #1147, #9022, #15645, #8915, #19196, #5673, #2651, #14347, #7718, #20926, #831, #7397, #3947, #13914, #6093, #5886, #9239, #4375, #20825, #18759, #15536, #2441, #14023, #2335, #10532, #5995, #4052, #936, #17153, #7503, #20602, #10640, #12382, #10857, #10963, #719, #15856, #4272, #14126, #7289, #14237, #12604, #12498, #1042, #20503, #12280, #18862, #5777, #17571, #18975, #2763, #9342, #15960, #20712, #4156, #10748, #17364, #2545, #17258, #9127, #15749, #7607, #19089, #57, #11069, #12708, #9763, #8133, #14450, #17783, #11283, #17675, #16281, #21137, #1456, #4689, #12921, #7820, #19614, #16069, #19722, #17881, #6408, #2975, #16388, #3294, #6309, #21350, #11387, #6517, #19510, #3074, #9657, #9553, #12815, #6201, #4587, #11501, #2869, #9454, #1563, #4791, #8031, #19300, #17988, #13133, #16172, #7922, #4905, #14662, #14764, #3184, #19405, #1349, #14551, #21243, #18098, #13022, #9867, #1245, #16492, #1674, #8245, #14874, #4485, #21030, #11181, #14980, #5327, #2202, #17021, #8788, #10087, #3501, #13246, #1789, #10404, #15193, #11928, #7053, #8677, #6625, #18202, #11719, #16708, #11611, #19835, #15301, #13353, #10191, #5011, #16813, #18311, #19942, #274, #20160, #13672, #9979, #18521, #13570, #2002, #15406, #2099, #488, #378, #3707, #3398, #16600, #6737, #1897, #20261, #8465, #5431, #12032, #18624, #8570, #13457, #15089, #5226, #6842, #3812, #8356, #167, #10294, #5119, #20050, #11825, #18419, #16917, #3606, #6948, #5648, #20579, #5539, #4130, #8997, #10720, #13999, #805, #17130, #7473, #3918, #7582, #5749, #15724, #12254, #19064, #12579, #15617, #9210, #20686, #15832, #7371, #12359, #18948, #18837, #693, #15510, #13887, #20798, #12145, #18734, #4247, #14103, #17336, #587, #5861, #1018, #4024, #2521, #9103, #17546, #10617, #5966, #911, #20365, #2416, #17233, #12468, #2310, #14211, #8892, #10833, #17441, #2626, #19173, #4351, #7263, #20477, #10935, #2736, #9316, #7155, #13777, #10508, #4564, #17757, #1223, #2843, #14738, #16145, #15933, #8002, #9427, #9633, #3159, #17958, #7794, #11040, #7897, #17651, #11362, #6384, #4455, #9526, #1430, #16045, #19274, #4767, #14635, #11256, #14427, #21220, #1122, #11472, #1325, #12995, #19691, #19587, #7693, #9737, #21007, #6489, #14524, #4877, #6069, #16358, #6176, #11153, #12786, #20901, #19379, #2947, #8107, #21110, #6281, #12896, #14322, #18069, #4666, #19485, #1536, #17856, #3049, #21320, #16251, #13107, #3265, #12681, #5091, #8328, #3373, #3683, #5298, #10167, #1868, #8219, #20131, #6711, #18493, #13645, #6814, #14950, #10269, #13541, #18599, #16886, #9840, #18283, #16572, #2070, #20231, #13327, #19807, #137, #5402, #13429, #7024, #12007, #20022, #3578, #16785, #10057, #8438, #16464, #1757, #1647, #11900, #14847, #11794, #19910, #4984, #22, #8646, #6598, #3472, #11692, #15274, #13219, #16680, #11583, #15062, #18175, #5196, #9950, #244, #18389, #1973, #8543, #15164, #353, #6916, #457, #7556, #7447, #16996, #5722, #666, #20338, #2175, #8760, #5619, #15481, #8861, #5513, #17419, #12112, #3992, #2494, #4102, #7232, #13858, #18704, #3890, #20555, #20446, #2600, #14182, #14075, #9180, #12228, #18811, #10481, #17101, #15806, #10585, #3782, #17310, #2281, #18918, #12438, #5829, #17206, #2385, #8968, #15593, #20658, #15697, #13752, #778, #10690, #7339, #7126, #19036, #9076, #12330, #13973, #883, #10372, #20772, #4221, #10804, #5940, #993, #15380, #12555, #558, #9714, #11124, #8083, #9291, #1403, #11014, #14398, #14294, #2710, #12653, #19248, #11339, #7770, #4430, #12760, #10908, #14713, #7871, #1297, #3026, #20880, #17624, #19560, #2816, #9400, #6148, #7666, #20980, #16018, #1200, #12970, #14607, #19458, #17729, #17520, #7978, #19349, #6360, #1509, #16118, #4539, #4741, #21191, #6464, #17933, #15906, #1098, #17830, #6045, #19150, #2923, #4325, #16226, #3128, #9503, #14500, #21083, #6256, #12868, #4642, #11233, #9608, #16335, #21290, #16658, #9814, #3556, #6681, #3447, #19774, #220, #1949, #9924, #5173, #1843, #11770, #1728, #13301, #19886, #4960, #14819, #738, #13191, #10145, #18045, #3239, #6788, #8412, #5062, #13080, #13406, #16761, #11559, #11666, #18256, #6893, #3343, #8518, #10031, #16543, #18365, #15036, #19995, #15144, #6570, #8301, #14926, #18146, #326, #13514, #19666, #16437, #4844, #11443, #1617, #108, #8190, #1164, #11405, #19315, #9676, #6535, #21367, #13152, #14467, #7839, #17589, #6115, #14781, #19527, #16300, #18008, #13041, #10979, #7736, #16083, #21049, #15982, #2781, #19631, #17695, #14570, #9367, #21156, #1262, #2887, #4607, #3094, #3203, #14366, #1473, #17899, #6327, #19740, #6425, #4811, #4706, #8049, #20945, #12726, #11090, #6217, #9780, #12833, #16405, #1582, #8153, #12941, #17800, #19423, #9573, #11199, #4501, #2990, #9471, #16190, #14681, #1368 ),
 ( #7939, #11302, #21259, #16512, #9994, #8377, #9888, #4924, #6966, #11630, #8484, #11521, #15107, #16619, #18224, #19962, #18439, #11945, #8262, #3626, #11843, #291, #7068, #400, #13589, #20071, #10208, #18114, #3310, #5029, #1808, #20177, #15000, #3726, #5343, #18539, #6860, #11739, #187, #3519, #5140, #10311, #1692, #14891, #16831, #13266, #13686, #78, #6645, #2019, #16935, #19852, #6754, #10106, #3417, #13478, #13372, #5243, #18329, #16728, #1916, #8587, #15210, #2118, #8697, #15320, #505, #11163, #4674, #1131, #1333, #12796, #7906, #7703, #4466, #11049, #4358, #14221, #7591, #5977, #12905, #4256, #10843, #17766, #6185, #17661, #14111, #19388, #14534, #19181, #19283, #2853, #9643, #17555, #19496, #10945, #21119, #2958, #1441, #6291, #20696, #14331, #20808, #11266, #17865, #2744, #2635, #9325, #3058, #9435, #16263, #5869, #16054, #7803, #14435, #20911, #12690, #12481, #12589, #19073, #9535, #17448, #1231, #15945, #9220, #15839, #1026, #6077, #21016, #4573, #16155, #257, #3170, #8229, #6722, #8339, #19702, #13117, #1546, #8118, #3384, #4887, #6824, #18401, #11703, #13440, #18082, #9850, #14750, #16370, #20032, #14858, #8012, #149, #21333, #1770, #16691, #10068, #6500, #9749, #34, #11485, #3482, #19923, #17967, #1660, #14962, #3276, #11372, #18295, #13339, #9963, #16477, #5102, #14645, #3589, #6608, #1880, #11805, #8448, #21229, #15073, #13230, #5208, #19820, #10175, #19599, #16796, #4996, #11595, #18186, #13005, #16582, #6394, #4775, #12016, #16899, #17005, #15175, #12341, #12125, #5523, #7241, #3692, #15285, #2396, #2081, #7033, #10385, #11910, #18609, #468, #8660, #17215, #18821, #2291, #15388, #363, #12238, #20240, #10595, #5731, #20348, #1984, #2186, #13655, #15602, #18928, #5412, #18504, #3793, #4111, #18713, #20563, #10700, #3901, #17112, #8872, #8770, #568, #8555, #7136, #6929, #5628, #13553, #10490, #13762, #10280, #20142, #5309, #15490, #676, #13869, #20457, #788, #4003, #8978, #7349, #13980, #7565, #1001, #10813, #17427, #12665, #14191, #9510, #6264, #20991, #16127, #5948, #19159, #2608, #4230, #1309, #17528, #17319, #9410, #9191, #11023, #4547, #19359, #15816, #12447, #9301, #19046, #12769, #7777, #5841, #10917, #2825, #20782, #20667, #6156, #16026, #19257, #12564, #1207, #2502, #12880, #2720, #14409, #21091, #11135, #9086, #17738, #4336, #7881, #15915, #19467, #7456, #2930, #1106, #7677, #14303, #892, #20886, #6054, #14508, #4439, #17634, #4650, #15705, #14085, #7, #14828, #16553, #12978, #3139, #11675, #11346, #16343, #19675, #21203, #6473, #9721, #4750, #5073, #6692, #11567, #3247, #9617, #118, #8091, #19894, #15045, #8202, #1519, #18266, #14934, #20005, #3455, #19569, #4969, #10041, #13309, #17942, #6368, #9823, #14721, #16666, #1738, #21301, #4857, #18156, #13088, #14618, #1852, #3355, #6581, #11453, #9933, #17838, #6797, #18053, #8311, #228, #8421, #3034, #13414, #16447, #11240, #1628, #16236, #1412, #7987, #13202, #19786, #334, #10152, #20113, #5282, #18796, #15257, #11885, #20216, #18374, #15574, #15365, #8742, #10464, #6900, #3665, #5603, #10249, #16872, #13630, #15152, #439, #2056, #8629, #20430, #650, #5494, #18580, #3563, #15466, #7007, #13837, #8953, #2160, #5384, #12209, #8844, #13955, #3978, #11778, #11989, #3768, #10568, #760, #10355, #13523, #16980, #7325, #544, #2370, #16769, #7112, #20321, #12095, #13737, #18688, #1956, #3875, #8526, #7214, #17084, #2266, #17192, #15682, #12314, #18904, #978, #10786, #4203, #868, #12747, #7431, #20754, #19234, #20867, #17404, #2586, #14059, #20643, #15893, #9165, #19337, #9492, #2800, #4524, #15789, #7540, #5814, #12423, #11111, #5926, #20541, #12643, #19018, #14167, #4418, #6137, #2477, #11000, #6031, #9277, #1282, #16005, #1188, #14279, #17611, #4088, #5706, #12538, #19131, #7758, #4311, #17714, #14384, #20968, #2694, #10894, #17503, #1083, #7653, #2912, #10676, #17296, #9387, #16105, #7860, #9060, #14488, #11838, #10204, #16212, #19847, #13366, #19443, #18324, #1803, #3514, #6749, #14995, #9595, #286, #17819, #395, #19957, #8479, #5024, #18434, #5339, #8371, #2015, #13473, #8582, #181, #5134, #11733, #11624, #14594, #7964, #6640, #13584, #4628, #11222, #3619, #6854, #10101, #21069, #20065, #15205, #18219, #16722, #1911, #10305, #3410, #20173, #15101, #9989, #6961, #5238, #16826, #11939, #72, #16613, #18534, #3722, #16931, #2113, #6242, #3011, #12855, #1389, #13261, #20378, #5551, #20273, #9115, #17035, #7384, #4258, #19075, #10846, #12157, #18745, #15315, #3826, #12483, #17244, #14010, #15736, #10735, #8692, #5445, #13788, #3933, #13682, #501, #17349, #15416, #12265, #7063, #18849, #10519, #922, #13899, #2427, #17141, #5760, #20698, #2322, #2532, #20590, #7487, #8902, #20489, #5660, #15520, #8799, #2216, #600, #14113, #12045, #18635, #12370, #817, #4037, #10414, #18958, #5871, #705, #10627, #9009, #17450, #7276, #7165, #15632, #4141, #17867, #19390, #6293, #9537, #2746, #12692, #6079, #7706, #11268, #21018, #12799, #20810, #6396, #1335, #13007, #14334, #20913, #14223, #3060, #10947, #7908, #19601, #4777, #11374, #19285, #4470, #9222, #19184, #2637, #11166, #14536, #9645, #4676, #15842, #5981, #11051, #17663, #7593, #1028, #16265, #9327, #6187, #12591, #4575, #2855, #15948, #9438, #16157, #1444, #4361, #21122, #12908, #17768, #17557, #19498, #8015, #2960, #14648, #1133, #16056, #1233, #7805, #21231, #14437, #16799, #20035, #13443, #153, #3387, #8232, #16585, #11600, #5211, #8121, #9752, #16694, #4891, #5312, #16375, #17970, #15076, #11810, #19705, #1663, #1773, #1549, #6725, #4999, #13342, #9966, #18189, #13120, #3485, #21336, #14861, #3280, #8343, #10073, #3592, #6504, #1883, #8451, #19927, #20145, #18404, #10178, #11706, #260, #14753, #3173, #18086, #37, #1987, #6612, #8558, #15179, #366, #5105, #14965, #13233, #18298, #6828, #6932, #11488, #9853, #13557, #16480, #19824, #3695, #11913, #5631, #18824, #7036, #3796, #5526, #16902, #3904, #571, #18717, #13765, #7139, #471, #15493, #8663, #2399, #12128, #2294, #10388, #12241, #792, #15391, #4006, #7244, #10598, #20351, #10493, #17115, #17009, #20243, #5415, #12019, #8981, #2084, #15288, #17218, #679, #8875, #18507, #15605, #7352, #2189, #13872, #20461, #10283, #13983, #13658, #20566, #5734, #18612, #8773, #13518, #16764, #9927, #19890, #13305, #14931, #18474, #6791, #19998, #6574, #13625, #8521, #20213, #112, #6685, #1, #10244, #18149, #15147, #5378, #11984, #18578, #5066, #11670, #16441, #4963, #9817, #18369, #329, #16869, #11882, #1620, #13195, #18260, #3451, #14822, #8193, #3661, #16547, #13409, #19777, #5176, #11562, #10036, #8306, #3347, #2051, #5278, #10148, #1847, #1732, #20108, #16662, #8625, #8415, #11773, #15040, #15249, #435, #224, #7002, #3559, #1952, #6896, #17398, #7535, #644, #13728, #8840, #14162, #755, #971, #20747, #13948, #18898, #4084, #3974, #2367, #5921, #17079, #12530, #7426, #16974, #5702, #7210, #20318, #2155, #8736, #5599, #15461, #13832, #5490, #2582, #12090, #10564, #2473, #10671, #20426, #12203, #18682, #3870, #20535, #18790, #9160, #3764, #14053, #15784, #17187, #8946, #10459, #2262, #10351, #15569, #15360, #17288, #7320, #9055, #12418, #5810, #12308, #15677, #863, #20637, #19012, #4195, #10781, #541, #7108, #19229, #1076, #7956, #4621, #14483, #12637, #11216, #4307, #14695, #19331, #3005, #1489, #17815, #10890, #9590, #4412, #9694, #11105, #8065, #9272, #1384, #10995, #14379, #14273, #2687, #17604, #2795, #11319, #7750, #9381, #12739, #17497, #21272, #7854, #1276, #16206, #20857, #15999, #19543, #1180, #20961, #6132, #12954, #19125, #4517, #17709, #17914, #6443, #2904, #7647, #9487, #15888, #16097, #16315, #6027, #21063 ) ),
 .UNSPECIFIED., .F., .F., .T. ) 
 B_SPLINE_SURFACE_WITH_KNOTS ( ( 2, 2 ),
 ( 3, 2, 2, 2, 2, 2, 2, 2, 2, 2, 2, 2, 2, 2, 2, 2, 2, 2, 2, 2, 2, 2, 2, 2, 2, 2, 2, 2, 2, 2, 2, 2, 2, 2, 2, 2, 2, 2, 2, 2, 2, 2, 2, 2, 2, 2, 2, 2, 2, 2, 2, 2, 2, 2, 2, 2, 2, 2, 2, 2, 2, 2, 2, 2, 2, 2, 2, 2, 2, 2, 2, 2, 2, 2, 2, 2, 2, 2, 2, 2, 2, 2, 2, 2, 2, 2, 2, 2, 2, 2, 2, 2, 2, 2, 2, 2, 2, 2, 2, 2, 2, 2, 2, 2, 2, 2, 2, 2, 2, 2, 2, 2, 2, 2, 2, 2, 2, 2, 2, 2, 2, 2, 2, 2, 2, 2, 2, 2, 2, 2, 2, 2, 2, 2, 2, 2, 2, 2, 2, 2, 2, 2, 2, 2, 2, 2, 2, 2, 2, 2, 2, 2, 2, 2, 2, 2, 2, 2, 2, 2, 2, 2, 2, 2, 2, 2, 2, 2, 2, 2, 2, 2, 2, 2, 2, 2, 2, 2, 2, 2, 2, 2, 2, 2, 2, 2, 2, 2, 2, 2, 2, 2, 2, 2, 2, 2, 2, 2, 2, 2, 2, 2, 2, 2, 2, 2, 2, 2, 2, 2, 2, 2, 2, 2, 2, 2, 2, 2, 2, 2, 2, 2, 2, 2, 2, 2, 2, 2, 2, 2, 2, 2, 2, 2, 2, 2, 2, 2, 2, 2, 2, 2, 2, 2, 2, 2, 2, 2, 2, 2, 2, 2, 2, 2, 2, 2, 2, 2, 2, 2, 2, 2, 2, 2, 2, 2, 2, 2, 2, 2, 2, 2, 2, 2, 2, 2, 2, 2, 2, 2, 2, 2, 2, 2, 2, 2, 2, 2, 2, 2, 2, 2, 2, 2, 2, 2, 2, 2, 2, 2, 2, 2, 2, 2, 2, 2, 2, 2, 2, 2, 2, 2, 2, 2, 2, 2, 2, 2, 2, 2, 2, 2, 2, 2, 2, 2, 2, 2, 2, 2, 2, 2, 2, 2, 2, 2, 2, 2, 2, 2, 2, 2, 2, 2, 2, 2, 2, 2, 2, 2, 2, 2, 2, 2, 2, 2, 2, 2, 2, 2, 2, 2, 2, 2, 2, 2, 2, 2, 2, 2, 2, 2, 2, 2, 2, 2, 2, 2, 2, 2, 2, 2, 2, 2, 2, 2, 2, 2, 2, 2, 2, 2, 2, 2, 2, 2, 2, 2, 2, 2, 2, 2, 2, 2, 2, 2, 2, 2, 2, 2, 2, 2, 2, 2, 2, 2, 2, 2, 2, 2, 2, 2, 2, 2, 2, 2, 2, 2, 2, 2, 2, 2, 2, 2, 2, 2, 2, 2, 2, 2, 2, 2, 2, 2, 2, 2, 2, 2, 2, 2, 2, 2, 2, 2, 2, 2, 2, 2, 2, 2, 2, 2, 2, 2, 2, 2, 2, 2, 2, 2, 2, 2, 2, 2, 2, 2, 2, 2, 2, 2, 2, 2, 2, 2, 2, 2, 2, 2, 2, 2, 2, 2, 2, 2, 2, 2, 2, 2, 2, 2, 2, 2, 3 ),
 ( 0.000000000000000000, 1.000000000000000000 ),
 ( 0.000000000000000000, 0.001953125000000000000, 0.003906250000000000000, 0.005859375000000000000, 0.007812500000000000000, 0.009765625000000000000, 0.01171875000000000000, 0.01367187500000000000, 0.01562500000000000000, 0.01757812500000000000, 0.01953125000000000000, 0.02148437500000000000, 0.02343750000000000000, 0.02539062500000000000, 0.02734375000000000000, 0.02929687500000000000, 0.03125000000000000000, 0.03320312500000000000, 0.03515625000000000000, 0.03710937500000000000, 0.03906250000000000000, 0.04101562500000000000, 0.04296875000000000000, 0.04492187500000000000, 0.04687500000000000000, 0.04882812500000000000, 0.05078125000000000000, 0.05273437500000000000, 0.05468750000000000000, 0.05664062500000000000, 0.05859375000000000000, 0.06054687500000000000, 0.06250000000000000000, 0.06445312500000000000, 0.06640625000000000000, 0.06835937500000000000, 0.07031250000000000000, 0.07226562500000000000, 0.07421875000000000000, 0.07617187500000000000, 0.07812500000000000000, 0.08007812500000000000, 0.08203125000000000000, 0.08398437500000000000, 0.08593750000000000000, 0.08789062500000000000, 0.08984375000000000000, 0.09179687500000000000, 0.09375000000000000000, 0.09570312500000000000, 0.09765625000000000000, 0.09960937500000000000, 0.1015625000000000000, 0.1035156250000000000, 0.1054687500000000000, 0.1074218750000000000, 0.1093750000000000000, 0.1113281250000000000, 0.1132812500000000000, 0.1152343750000000000, 0.1171875000000000000, 0.1191406250000000000, 0.1210937500000000000, 0.1230468750000000000, 0.1250000000000000000, 0.1269531250000000000, 0.1289062500000000000, 0.1308593750000000000, 0.1328125000000000000, 0.1347656250000000000, 0.1367187500000000000, 0.1386718750000000000, 0.1406250000000000000, 0.1425781250000000000, 0.1445312500000000000, 0.1464843750000000000, 0.1484375000000000000, 0.1503906250000000000, 0.1523437500000000000, 0.1542968750000000000, 0.1562500000000000000, 0.1582031250000000000, 0.1601562500000000000, 0.1621093750000000000, 0.1640625000000000000, 0.1660156250000000000, 0.1679687500000000000, 0.1699218750000000000, 0.1718750000000000000, 0.1738281250000000000, 0.1757812500000000000, 0.1777343750000000000, 0.1796875000000000000, 0.1816406250000000000, 0.1835937500000000000, 0.1855468750000000000, 0.1875000000000000000, 0.1894531250000000000, 0.1914062500000000000, 0.1933593750000000000, 0.1953125000000000000, 0.1972656250000000000, 0.1992187500000000000, 0.2011718750000000000, 0.2031250000000000000, 0.2050781250000000000, 0.2070312500000000000, 0.2089843750000000000, 0.2109375000000000000, 0.2128906250000000000, 0.2148437500000000000, 0.2167968750000000000, 0.2187500000000000000, 0.2207031250000000000, 0.2226562500000000000, 0.2246093750000000000, 0.2265625000000000000, 0.2285156250000000000, 0.2304687500000000000, 0.2324218750000000000, 0.2343750000000000000, 0.2363281250000000000, 0.2382812500000000000, 0.2402343750000000000, 0.2421875000000000000, 0.2441406250000000000, 0.2460937500000000000, 0.2480468750000000000, 0.2500000000000000000, 0.2519531250000000000, 0.2539062500000000000, 0.2558593750000000000, 0.2578125000000000000, 0.2597656250000000000, 0.2617187500000000000, 0.2636718750000000000, 0.2656250000000000000, 0.2675781250000000000, 0.2695312500000000000, 0.2714843750000000000, 0.2734375000000000000, 0.2753906250000000000, 0.2773437500000000000, 0.2792968750000000000, 0.2812500000000000000, 0.2832031250000000000, 0.2851562500000000000, 0.2871093750000000000, 0.2890625000000000000, 0.2910156250000000000, 0.2929687500000000000, 0.2949218750000000000, 0.2968750000000000000, 0.2988281250000000000, 0.3007812500000000000, 0.3027343750000000000, 0.3046875000000000000, 0.3066406250000000000, 0.3085937500000000000, 0.3105468750000000000, 0.3125000000000000000, 0.3144531250000000000, 0.3164062500000000000, 0.3183593750000000000, 0.3203125000000000000, 0.3222656250000000000, 0.3242187500000000000, 0.3261718750000000000, 0.3281250000000000000, 0.3300781250000000000, 0.3320312500000000000, 0.3339843750000000000, 0.3359375000000000000, 0.3378906250000000000, 0.3398437500000000000, 0.3417968750000000000, 0.3437500000000000000, 0.3457031250000000000, 0.3476562500000000000, 0.3496093750000000000, 0.3515625000000000000, 0.3535156250000000000, 0.3554687500000000000, 0.3574218750000000000, 0.3593750000000000000, 0.3613281250000000000, 0.3632812500000000000, 0.3652343750000000000, 0.3671875000000000000, 0.3691406250000000000, 0.3710937500000000000, 0.3730468750000000000, 0.3750000000000000000, 0.3769531250000000000, 0.3789062500000000000, 0.3808593750000000000, 0.3828125000000000000, 0.3847656250000000000, 0.3867187500000000000, 0.3886718750000000000, 0.3906250000000000000, 0.3925781250000000000, 0.3945312500000000000, 0.3964843750000000000, 0.3984375000000000000, 0.4003906250000000000, 0.4023437500000000000, 0.4042968750000000000, 0.4062500000000000000, 0.4082031250000000000, 0.4101562500000000000, 0.4121093750000000000, 0.4140625000000000000, 0.4160156250000000000, 0.4179687500000000000, 0.4199218750000000000, 0.4218750000000000000, 0.4238281250000000000, 0.4257812500000000000, 0.4277343750000000000, 0.4296875000000000000, 0.4316406250000000000, 0.4335937500000000000, 0.4355468750000000000, 0.4375000000000000000, 0.4394531250000000000, 0.4414062500000000000, 0.4433593750000000000, 0.4453125000000000000, 0.4472656250000000000, 0.4492187500000000000, 0.4511718750000000000, 0.4531250000000000000, 0.4550781250000000000, 0.4570312500000000000, 0.4589843750000000000, 0.4609375000000000000, 0.4628906250000000000, 0.4648437500000000000, 0.4667968750000000000, 0.4687500000000000000, 0.4707031250000000000, 0.4726562500000000000, 0.4746093750000000000, 0.4765625000000000000, 0.4785156250000000000, 0.4804687500000000000, 0.4824218750000000000, 0.4843750000000000000, 0.4863281250000000000, 0.4882812500000000000, 0.4902343750000000000, 0.4921875000000000000, 0.4941406250000000000, 0.4960937500000000000, 0.4980468750000000000, 0.5000000000000000000, 0.5019531250000000000, 0.5039062500000000000, 0.5058593750000000000, 0.5078125000000000000, 0.5097656250000000000, 0.5117187500000000000, 0.5136718750000000000, 0.5156250000000000000, 0.5175781250000000000, 0.5195312500000000000, 0.5214843750000000000, 0.5234375000000000000, 0.5253906250000000000, 0.5273437500000000000, 0.5292968750000000000, 0.5312500000000000000, 0.5332031250000000000, 0.5351562500000000000, 0.5371093750000000000, 0.5390625000000000000, 0.5410156250000000000, 0.5429687500000000000, 0.5449218750000000000, 0.5468750000000000000, 0.5488281250000000000, 0.5507812500000000000, 0.5527343750000000000, 0.5546875000000000000, 0.5566406250000000000, 0.5585937500000000000, 0.5605468750000000000, 0.5625000000000000000, 0.5644531250000000000, 0.5664062500000000000, 0.5683593750000000000, 0.5703125000000000000, 0.5722656250000000000, 0.5742187500000000000, 0.5761718750000000000, 0.5781250000000000000, 0.5800781250000000000, 0.5820312500000000000, 0.5839843750000000000, 0.5859375000000000000, 0.5878906250000000000, 0.5898437500000000000, 0.5917968750000000000, 0.5937500000000000000, 0.5957031250000000000, 0.5976562500000000000, 0.5996093750000000000, 0.6015625000000000000, 0.6035156250000000000, 0.6054687500000000000, 0.6074218750000000000, 0.6093750000000000000, 0.6113281250000000000, 0.6132812500000000000, 0.6152343750000000000, 0.6171875000000000000, 0.6191406250000000000, 0.6210937500000000000, 0.6230468750000000000, 0.6250000000000000000, 0.6269531250000000000, 0.6289062500000000000, 0.6308593750000000000, 0.6328125000000000000, 0.6347656250000000000, 0.6367187500000000000, 0.6386718750000000000, 0.6406250000000000000, 0.6425781250000000000, 0.6445312500000000000, 0.6464843750000000000, 0.6484375000000000000, 0.6503906250000000000, 0.6523437500000000000, 0.6542968750000000000, 0.6562500000000000000, 0.6582031250000000000, 0.6601562500000000000, 0.6621093750000000000, 0.6640625000000000000, 0.6660156250000000000, 0.6679687500000000000, 0.6699218750000000000, 0.6718750000000000000, 0.6738281250000000000, 0.6757812500000000000, 0.6777343750000000000, 0.6796875000000000000, 0.6816406250000000000, 0.6835937500000000000, 0.6855468750000000000, 0.6875000000000000000, 0.6894531250000000000, 0.6914062500000000000, 0.6933593750000000000, 0.6953125000000000000, 0.6972656250000000000, 0.6992187500000000000, 0.7011718750000000000, 0.7031250000000000000, 0.7050781250000000000, 0.7070312500000000000, 0.7089843750000000000, 0.7109375000000000000, 0.7128906250000000000, 0.7148437500000000000, 0.7167968750000000000, 0.7187500000000000000, 0.7207031250000000000, 0.7226562500000000000, 0.7246093750000000000, 0.7265625000000000000, 0.7285156250000000000, 0.7304687500000000000, 0.7324218750000000000, 0.7343750000000000000, 0.7363281250000000000, 0.7382812500000000000, 0.7402343750000000000, 0.7421875000000000000, 0.7441406250000000000, 0.7460937500000000000, 0.7480468750000000000, 0.7500000000000000000, 0.7519531250000000000, 0.7539062500000000000, 0.7558593750000000000, 0.7578125000000000000, 0.7597656250000000000, 0.7617187500000000000, 0.7636718750000000000, 0.7656250000000000000, 0.7675781250000000000, 0.7695312500000000000, 0.7714843750000000000, 0.7734375000000000000, 0.7753906250000000000, 0.7773437500000000000, 0.7792968750000000000, 0.7812500000000000000, 0.7832031250000000000, 0.7851562500000000000, 0.7871093750000000000, 0.7890625000000000000, 0.7910156250000000000, 0.7929687500000000000, 0.7949218750000000000, 0.7968750000000000000, 0.7988281250000000000, 0.8007812500000000000, 0.8027343750000000000, 0.8046875000000000000, 0.8066406250000000000, 0.8085937500000000000, 0.8105468750000000000, 0.8125000000000000000, 0.8144531250000000000, 0.8164062500000000000, 0.8183593750000000000, 0.8203125000000000000, 0.8222656250000000000, 0.8242187500000000000, 0.8261718750000000000, 0.8281250000000000000, 0.8300781250000000000, 0.8320312500000000000, 0.8339843750000000000, 0.8359375000000000000, 0.8378906250000000000, 0.8398437500000000000, 0.8417968750000000000, 0.8437500000000000000, 0.8457031250000000000, 0.8476562500000000000, 0.8496093750000000000, 0.8515625000000000000, 0.8535156250000000000, 0.8554687500000000000, 0.8574218750000000000, 0.8593750000000000000, 0.8613281250000000000, 0.8632812500000000000, 0.8652343750000000000, 0.8671875000000000000, 0.8691406250000000000, 0.8710937500000000000, 0.8730468750000000000, 0.8750000000000000000, 0.8769531250000000000, 0.8789062500000000000, 0.8808593750000000000, 0.8828125000000000000, 0.8847656250000000000, 0.8867187500000000000, 0.8886718750000000000, 0.8906250000000000000, 0.8925781250000000000, 0.8945312500000000000, 0.8964843750000000000, 0.8984375000000000000, 0.9003906250000000000, 0.9023437500000000000, 0.9042968750000000000, 0.9062500000000000000, 0.9082031250000000000, 0.9101562500000000000, 0.9121093750000000000, 0.9140625000000000000, 0.9160156250000000000, 0.9179687500000000000, 0.9199218750000000000, 0.9218750000000000000, 0.9238281250000000000, 0.9257812500000000000, 0.9277343750000000000, 0.9296875000000000000, 0.9316406250000000000, 0.9335937500000000000, 0.9355468750000000000, 0.9375000000000000000, 0.9394531250000000000, 0.9414062500000000000, 0.9433593750000000000, 0.9453125000000000000, 0.9472656250000000000, 0.9492187500000000000, 0.9511718750000000000, 0.9531250000000000000, 0.9550781250000000000, 0.9570312500000000000, 0.9589843750000000000, 0.9609375000000000000, 0.9628906250000000000, 0.9648437500000000000, 0.9667968750000000000, 0.9687500000000000000, 0.9707031250000000000, 0.9726562500000000000, 0.9746093750000000000, 0.9765625000000000000, 0.9785156250000000000, 0.9791718287086115247 ),
 .UNSPECIFIED. ) 
 GEOMETRIC_REPRESENTATION_ITEM ( )  RATIONAL_B_SPLINE_SURFACE ( (
 ( 1.000000000000000000, 0.9807852804032304306, 1.000000000000000000, 0.9807852804032304306, 1.000000000000000000, 0.9807852804032304306, 1.000000000000000000, 0.9807852804032304306, 1.000000000000000000, 0.9807852804032304306, 1.000000000000000000, 0.9807852804032304306, 1.000000000000000000, 0.9807852804032304306, 1.000000000000000000, 0.9807852804032304306, 1.000000000000000000, 0.9807852804032304306, 1.000000000000000000, 0.9807852804032304306, 1.000000000000000000, 0.9807852804032304306, 1.000000000000000000, 0.9807852804032304306, 1.000000000000000000, 0.9807852804032304306, 1.000000000000000000, 0.9807852804032304306, 1.000000000000000000, 0.9807852804032304306, 1.000000000000000000, 0.9807852804032304306, 1.000000000000000000, 0.9807852804032304306, 1.000000000000000000, 0.9807852804032304306, 1.000000000000000000, 0.9807852804032304306, 1.000000000000000000, 0.9807852804032304306, 1.000000000000000000, 0.9807852804032304306, 1.000000000000000000, 0.9807852804032304306, 1.000000000000000000, 0.9807852804032304306, 1.000000000000000000, 0.9807852804032304306, 1.000000000000000000, 0.9807852804032304306, 1.000000000000000000, 0.9807852804032304306, 1.000000000000000000, 0.9807852804032304306, 1.000000000000000000, 0.9807852804032304306, 1.000000000000000000, 0.9807852804032304306, 1.000000000000000000, 0.9807852804032304306, 1.000000000000000000, 0.9807852804032304306, 1.000000000000000000, 0.9807852804032304306, 1.000000000000000000, 0.9807852804032304306, 1.000000000000000000, 0.9807852804032304306, 1.000000000000000000, 0.9807852804032304306, 1.000000000000000000, 0.9807852804032304306, 1.000000000000000000, 0.9807852804032304306, 1.000000000000000000, 0.9807852804032304306, 1.000000000000000000, 0.9807852804032304306, 1.000000000000000000, 0.9807852804032304306, 1.000000000000000000, 0.9807852804032304306, 1.000000000000000000, 0.9807852804032304306, 1.000000000000000000, 0.9807852804032304306, 1.000000000000000000, 0.9807852804032304306, 1.000000000000000000, 0.9807852804032304306, 1.000000000000000000, 0.9807852804032304306, 1.000000000000000000, 0.9807852804032304306, 1.000000000000000000, 0.9807852804032304306, 1.000000000000000000, 0.9807852804032304306, 1.000000000000000000, 0.9807852804032304306, 1.000000000000000000, 0.9807852804032304306, 1.000000000000000000, 0.9807852804032304306, 1.000000000000000000, 0.9807852804032304306, 1.000000000000000000, 0.9807852804032304306, 1.000000000000000000, 0.9807852804032304306, 1.000000000000000000, 0.9807852804032304306, 1.000000000000000000, 0.9807852804032304306, 1.000000000000000000, 0.9807852804032304306, 1.000000000000000000, 0.9807852804032304306, 1.000000000000000000, 0.9807852804032304306, 1.000000000000000000, 0.9807852804032304306, 1.000000000000000000, 0.9807852804032304306, 1.000000000000000000, 0.9807852804032304306, 1.000000000000000000, 0.9807852804032304306, 1.000000000000000000, 0.9807852804032304306, 1.000000000000000000, 0.9807852804032304306, 1.000000000000000000, 0.9807852804032304306, 1.000000000000000000, 0.9807852804032304306, 1.000000000000000000, 0.9807852804032304306, 1.000000000000000000, 0.9807852804032304306, 1.000000000000000000, 0.9807852804032304306, 1.000000000000000000, 0.9807852804032304306, 1.000000000000000000, 0.9807852804032304306, 1.000000000000000000, 0.9807852804032304306, 1.000000000000000000, 0.9807852804032304306, 1.000000000000000000, 0.9807852804032304306, 1.000000000000000000, 0.9807852804032304306, 1.000000000000000000, 0.9807852804032304306, 1.000000000000000000, 0.9807852804032304306, 1.000000000000000000, 0.9807852804032304306, 1.000000000000000000, 0.9807852804032304306, 1.000000000000000000, 0.9807852804032304306, 1.000000000000000000, 0.9807852804032304306, 1.000000000000000000, 0.9807852804032304306, 1.000000000000000000, 0.9807852804032304306, 1.000000000000000000, 0.9807852804032304306, 1.000000000000000000, 0.9807852804032304306, 1.000000000000000000, 0.9807852804032304306, 1.000000000000000000, 0.9807852804032304306, 1.000000000000000000, 0.9807852804032304306, 1.000000000000000000, 0.9807852804032304306, 1.000000000000000000, 0.9807852804032304306, 1.000000000000000000, 0.9807852804032304306, 1.000000000000000000, 0.9807852804032304306, 1.000000000000000000, 0.9807852804032304306, 1.000000000000000000, 0.9807852804032304306, 1.000000000000000000, 0.9807852804032304306, 1.000000000000000000, 0.9807852804032304306, 1.000000000000000000, 0.9807852804032304306, 1.000000000000000000, 0.9807852804032304306, 1.000000000000000000, 0.9807852804032304306, 1.000000000000000000, 0.9807852804032304306, 1.000000000000000000, 0.9807852804032304306, 1.000000000000000000, 0.9807852804032304306, 1.000000000000000000, 0.9807852804032304306, 1.000000000000000000, 0.9807852804032304306, 1.000000000000000000, 0.9807852804032304306, 1.000000000000000000, 0.9807852804032304306, 1.000000000000000000, 0.9807852804032304306, 1.000000000000000000, 0.9807852804032304306, 1.000000000000000000, 0.9807852804032304306, 1.000000000000000000, 0.9807852804032304306, 1.000000000000000000, 0.9807852804032304306, 1.000000000000000000, 0.9807852804032304306, 1.000000000000000000, 0.9807852804032304306, 1.000000000000000000, 0.9807852804032304306, 1.000000000000000000, 0.9807852804032304306, 1.000000000000000000, 0.9807852804032304306, 1.000000000000000000, 0.9807852804032304306, 1.000000000000000000, 0.9807852804032304306, 1.000000000000000000, 0.9807852804032304306, 1.000000000000000000, 0.9807852804032304306, 1.000000000000000000, 0.9807852804032304306, 1.000000000000000000, 0.9807852804032304306, 1.000000000000000000, 0.9807852804032304306, 1.000000000000000000, 0.9807852804032304306, 1.000000000000000000, 0.9807852804032304306, 1.000000000000000000, 0.9807852804032304306, 1.000000000000000000, 0.9807852804032304306, 1.000000000000000000, 0.9807852804032304306, 1.000000000000000000, 0.9807852804032304306, 1.000000000000000000, 0.9807852804032304306, 1.000000000000000000, 0.9807852804032304306, 1.000000000000000000, 0.9807852804032304306, 1.000000000000000000, 0.9807852804032304306, 1.000000000000000000, 0.9807852804032304306, 1.000000000000000000, 0.9807852804032304306, 1.000000000000000000, 0.9807852804032304306, 1.000000000000000000, 0.9807852804032304306, 1.000000000000000000, 0.9807852804032304306, 1.000000000000000000, 0.9807852804032304306, 1.000000000000000000, 0.9807852804032304306, 1.000000000000000000, 0.9807852804032304306, 1.000000000000000000, 0.9807852804032304306, 1.000000000000000000, 0.9807852804032304306, 1.000000000000000000, 0.9807852804032304306, 1.000000000000000000, 0.9807852804032304306, 1.000000000000000000, 0.9807852804032304306, 1.000000000000000000, 0.9807852804032304306, 1.000000000000000000, 0.9807852804032304306, 1.000000000000000000, 0.9807852804032304306, 1.000000000000000000, 0.9807852804032304306, 1.000000000000000000, 0.9807852804032304306, 1.000000000000000000, 0.9807852804032304306, 1.000000000000000000, 0.9807852804032304306, 1.000000000000000000, 0.9807852804032304306, 1.000000000000000000, 0.9807852804032304306, 1.000000000000000000, 0.9807852804032304306, 1.000000000000000000, 0.9807852804032304306, 1.000000000000000000, 0.9807852804032304306, 1.000000000000000000, 0.9807852804032304306, 1.000000000000000000, 0.9807852804032304306, 1.000000000000000000, 0.9807852804032304306, 1.000000000000000000, 0.9807852804032304306, 1.000000000000000000, 0.9807852804032304306, 1.000000000000000000, 0.9807852804032304306, 1.000000000000000000, 0.9807852804032304306, 1.000000000000000000, 0.9807852804032304306, 1.000000000000000000, 0.9807852804032304306, 1.000000000000000000, 0.9807852804032304306, 1.000000000000000000, 0.9807852804032304306, 1.000000000000000000, 0.9807852804032304306, 1.000000000000000000, 0.9807852804032304306, 1.000000000000000000, 0.9807852804032304306, 1.000000000000000000, 0.9807852804032304306, 1.000000000000000000, 0.9807852804032304306, 1.000000000000000000, 0.9807852804032304306, 1.000000000000000000, 0.9807852804032304306, 1.000000000000000000, 0.9807852804032304306, 1.000000000000000000, 0.9807852804032304306, 1.000000000000000000, 0.9807852804032304306, 1.000000000000000000, 0.9807852804032304306, 1.000000000000000000, 0.9807852804032304306, 1.000000000000000000, 0.9807852804032304306, 1.000000000000000000, 0.9807852804032304306, 1.000000000000000000, 0.9807852804032304306, 1.000000000000000000, 0.9807852804032304306, 1.000000000000000000, 0.9807852804032304306, 1.000000000000000000, 0.9807852804032304306, 1.000000000000000000, 0.9807852804032304306, 1.000000000000000000, 0.9807852804032304306, 1.000000000000000000, 0.9807852804032304306, 1.000000000000000000, 0.9807852804032304306, 1.000000000000000000, 0.9807852804032304306, 1.000000000000000000, 0.9807852804032304306, 1.000000000000000000, 0.9807852804032304306, 1.000000000000000000, 0.9807852804032304306, 1.000000000000000000, 0.9807852804032304306, 1.000000000000000000, 0.9807852804032304306, 1.000000000000000000, 0.9807852804032304306, 1.000000000000000000, 0.9807852804032304306, 1.000000000000000000, 0.9807852804032304306, 1.000000000000000000, 0.9807852804032304306, 1.000000000000000000, 0.9807852804032304306, 1.000000000000000000, 0.9807852804032304306, 1.000000000000000000, 0.9807852804032304306, 1.000000000000000000, 0.9807852804032304306, 1.000000000000000000, 0.9807852804032304306, 1.000000000000000000, 0.9807852804032304306, 1.000000000000000000, 0.9807852804032304306, 1.000000000000000000, 0.9807852804032304306, 1.000000000000000000, 0.9807852804032304306, 1.000000000000000000, 0.9807852804032304306, 1.000000000000000000, 0.9807852804032304306, 1.000000000000000000, 0.9807852804032304306, 1.000000000000000000, 0.9807852804032304306, 1.000000000000000000, 0.9807852804032304306, 1.000000000000000000, 0.9807852804032304306, 1.000000000000000000, 0.9807852804032304306, 1.000000000000000000, 0.9807852804032304306, 1.000000000000000000, 0.9807852804032304306, 1.000000000000000000, 0.9807852804032304306, 1.000000000000000000, 0.9807852804032304306, 1.000000000000000000, 0.9807852804032304306, 1.000000000000000000, 0.9807852804032304306, 1.000000000000000000, 0.9807852804032304306, 1.000000000000000000, 0.9807852804032304306, 1.000000000000000000, 0.9807852804032304306, 1.000000000000000000, 0.9807852804032304306, 1.000000000000000000, 0.9807852804032304306, 1.000000000000000000, 0.9807852804032304306, 1.000000000000000000, 0.9807852804032304306, 1.000000000000000000, 0.9807852804032304306, 1.000000000000000000, 0.9807852804032304306, 1.000000000000000000, 0.9807852804032304306, 1.000000000000000000, 0.9807852804032304306, 1.000000000000000000, 0.9807852804032304306, 1.000000000000000000, 0.9807852804032304306, 1.000000000000000000, 0.9807852804032304306, 1.000000000000000000, 0.9807852804032304306, 1.000000000000000000, 0.9807852804032304306, 1.000000000000000000, 0.9807852804032304306, 1.000000000000000000, 0.9807852804032304306, 1.000000000000000000, 0.9807852804032304306, 1.000000000000000000, 0.9807852804032304306, 1.000000000000000000, 0.9807852804032304306, 1.000000000000000000, 0.9807852804032304306, 1.000000000000000000, 0.9807852804032304306, 1.000000000000000000, 0.9807852804032304306, 1.000000000000000000, 0.9807852804032304306, 1.000000000000000000, 0.9807852804032304306, 1.000000000000000000, 0.9807852804032304306, 1.000000000000000000, 0.9807852804032304306, 1.000000000000000000, 0.9807852804032304306, 1.000000000000000000, 0.9807852804032304306, 1.000000000000000000, 0.9807852804032304306, 1.000000000000000000, 0.9807852804032304306, 1.000000000000000000, 0.9807852804032304306, 1.000000000000000000, 0.9807852804032304306, 1.000000000000000000, 0.9807852804032304306, 1.000000000000000000, 0.9807852804032304306, 1.000000000000000000, 0.9807852804032304306, 1.000000000000000000, 0.9807852804032304306, 1.000000000000000000, 0.9807852804032304306, 1.000000000000000000, 0.9807852804032304306, 1.000000000000000000, 0.9807852804032304306, 1.000000000000000000, 0.9807852804032304306, 1.000000000000000000, 0.9807852804032304306, 1.000000000000000000, 0.9807852804032304306, 1.000000000000000000, 0.9807852804032304306, 1.000000000000000000, 0.9807852804032304306, 1.000000000000000000, 0.9807852804032304306, 1.000000000000000000, 0.9807852804032304306, 1.000000000000000000, 0.9807852804032304306, 1.000000000000000000, 0.9807852804032304306, 1.000000000000000000, 0.9807852804032304306, 1.000000000000000000, 0.9807852804032304306, 1.000000000000000000, 0.9807852804032304306, 1.000000000000000000, 0.9807852804032304306, 1.000000000000000000, 0.9807852804032304306, 1.000000000000000000, 0.9807852804032304306, 1.000000000000000000, 0.9807852804032304306, 1.000000000000000000, 0.9807852804032304306, 1.000000000000000000, 0.9807852804032304306, 1.000000000000000000, 0.9807852804032304306, 1.000000000000000000, 0.9807852804032304306, 1.000000000000000000, 0.9807852804032304306, 1.000000000000000000, 0.9807852804032304306, 1.000000000000000000, 0.9807852804032304306, 1.000000000000000000, 0.9807852804032304306, 1.000000000000000000, 0.9807852804032304306, 1.000000000000000000, 0.9807852804032304306, 1.000000000000000000, 0.9807852804032304306, 1.000000000000000000, 0.9807852804032304306, 1.000000000000000000, 0.9807852804032304306, 1.000000000000000000, 0.9807852804032304306, 1.000000000000000000, 0.9807852804032304306, 1.000000000000000000, 0.9807852804032304306, 1.000000000000000000, 0.9807852804032304306, 1.000000000000000000, 0.9807852804032304306, 1.000000000000000000, 0.9807852804032304306, 1.000000000000000000, 0.9807852804032304306, 1.000000000000000000, 0.9807852804032304306, 1.000000000000000000, 0.9807852804032304306, 1.000000000000000000, 0.9807852804032304306, 1.000000000000000000, 0.9807852804032304306, 1.000000000000000000, 0.9807852804032304306, 1.000000000000000000, 0.9807852804032304306, 1.000000000000000000, 0.9807852804032304306, 1.000000000000000000, 0.9807852804032304306, 1.000000000000000000, 0.9807852804032304306, 1.000000000000000000, 0.9807852804032304306, 1.000000000000000000, 0.9807852804032304306, 1.000000000000000000, 0.9807852804032304306, 1.000000000000000000, 0.9807852804032304306, 1.000000000000000000, 0.9807852804032304306, 1.000000000000000000, 0.9807852804032304306, 1.000000000000000000, 0.9807852804032304306, 1.000000000000000000, 0.9807852804032304306, 1.000000000000000000, 0.9807852804032304306, 1.000000000000000000, 0.9807852804032304306, 1.000000000000000000, 0.9807852804032304306, 1.000000000000000000, 0.9807852804032304306, 1.000000000000000000, 0.9807852804032304306, 1.000000000000000000, 0.9807852804032304306, 1.000000000000000000, 0.9807852804032304306, 1.000000000000000000, 0.9807852804032304306, 1.000000000000000000, 0.9807852804032304306, 1.000000000000000000, 0.9807852804032304306, 1.000000000000000000, 0.9807852804032304306, 1.000000000000000000, 0.9807852804032304306, 1.000000000000000000, 0.9807852804032304306, 1.000000000000000000, 0.9807852804032304306, 1.000000000000000000, 0.9807852804032304306, 1.000000000000000000, 0.9807852804032304306, 1.000000000000000000, 0.9807852804032304306, 1.000000000000000000, 0.9807852804032304306, 1.000000000000000000, 0.9807852804032304306, 1.000000000000000000, 0.9807852804032304306, 1.000000000000000000, 0.9807852804032304306, 1.000000000000000000, 0.9807852804032304306, 1.000000000000000000, 0.9807852804032304306, 1.000000000000000000, 0.9807852804032304306, 1.000000000000000000, 0.9807852804032304306, 1.000000000000000000, 0.9807852804032304306, 1.000000000000000000, 0.9807852804032304306, 1.000000000000000000, 0.9807852804032304306, 1.000000000000000000, 0.9807852804032304306, 1.000000000000000000, 0.9807852804032304306, 1.000000000000000000, 0.9807852804032304306, 1.000000000000000000, 0.9807852804032304306, 1.000000000000000000, 0.9807852804032304306, 1.000000000000000000, 0.9807852804032304306, 1.000000000000000000, 0.9807852804032304306, 1.000000000000000000, 0.9807852804032304306, 1.000000000000000000, 0.9807852804032304306, 1.000000000000000000, 0.9807852804032304306, 1.000000000000000000, 0.9807852804032304306, 1.000000000000000000, 0.9807852804032304306, 1.000000000000000000, 0.9807852804032304306, 1.000000000000000000, 0.9807852804032304306, 1.000000000000000000, 0.9807852804032304306, 1.000000000000000000, 0.9807852804032304306, 1.000000000000000000, 0.9807852804032304306, 1.000000000000000000, 0.9807852804032304306, 1.000000000000000000, 0.9807852804032304306, 1.000000000000000000, 0.9807852804032304306, 1.000000000000000000, 0.9807852804032304306, 1.000000000000000000, 0.9807852804032304306, 1.000000000000000000, 0.9807852804032304306, 1.000000000000000000, 0.9807852804032304306, 1.000000000000000000, 0.9807852804032304306, 1.000000000000000000, 0.9807852804032304306, 1.000000000000000000, 0.9807852804032304306, 1.000000000000000000, 0.9807852804032304306, 1.000000000000000000, 0.9807852804032304306, 1.000000000000000000, 0.9807852804032304306, 1.000000000000000000, 0.9807852804032304306, 1.000000000000000000, 0.9807852804032304306, 1.000000000000000000, 0.9807852804032304306, 1.000000000000000000, 0.9807852804032304306, 1.000000000000000000, 0.9807852804032304306, 1.000000000000000000, 0.9807852804032304306, 1.000000000000000000, 0.9807852804032304306, 1.000000000000000000, 0.9807852804032304306, 1.000000000000000000, 0.9807852804032304306, 1.000000000000000000, 0.9807852804032304306, 1.000000000000000000, 0.9807852804032304306, 1.000000000000000000, 0.9807852804032304306, 1.000000000000000000, 0.9807852804032304306, 1.000000000000000000, 0.9807852804032304306, 1.000000000000000000, 0.9807852804032304306, 1.000000000000000000, 0.9807852804032304306, 1.000000000000000000, 0.9807852804032304306, 1.000000000000000000, 0.9807852804032304306, 1.000000000000000000, 0.9807852804032304306, 1.000000000000000000, 0.9807852804032304306, 1.000000000000000000, 0.9807852804032304306, 1.000000000000000000, 0.9807852804032304306, 1.000000000000000000, 0.9807852804032304306, 1.000000000000000000, 0.9807852804032304306, 1.000000000000000000, 0.9807852804032304306, 1.000000000000000000, 0.9807852804032304306, 1.000000000000000000, 0.9807852804032304306, 1.000000000000000000, 0.9807852804032304306, 1.000000000000000000, 0.9807852804032304306, 1.000000000000000000, 0.9807852804032304306, 1.000000000000000000, 0.9807852804032304306, 1.000000000000000000, 0.9807852804032304306, 1.000000000000000000, 0.9807852804032304306, 1.000000000000000000, 0.9807852804032304306, 1.000000000000000000, 0.9807852804032304306, 1.000000000000000000, 0.9807852804032304306, 1.000000000000000000, 0.9807852804032304306, 1.000000000000000000, 0.9807852804032304306, 1.000000000000000000, 0.9807852804032304306, 1.000000000000000000, 0.9807852804032304306, 1.000000000000000000, 0.9807852804032304306, 1.000000000000000000, 0.9807852804032304306, 1.000000000000000000, 0.9807852804032304306, 1.000000000000000000, 0.9807852804032304306, 1.000000000000000000, 0.9807852804032304306, 1.000000000000000000, 0.9807852804032304306, 1.000000000000000000, 0.9807852804032304306, 1.000000000000000000, 0.9807852804032304306, 1.000000000000000000, 0.9807852804032304306, 1.000000000000000000, 0.9807852804032304306, 1.000000000000000000, 0.9807852804032304306, 1.000000000000000000, 0.9807852804032304306, 1.000000000000000000, 0.9807852804032304306, 1.000000000000000000, 0.9807852804032304306, 1.000000000000000000, 0.9807852804032304306, 1.000000000000000000, 0.9807852804032304306, 1.000000000000000000, 0.9807852804032304306, 1.000000000000000000, 0.9807852804032304306, 1.000000000000000000, 0.9807852804032304306, 1.000000000000000000, 0.9807852804032304306, 1.000000000000000000, 0.9807852804032304306, 1.000000000000000000, 0.9807852804032304306, 1.000000000000000000, 0.9807852804032304306, 1.000000000000000000, 0.9807852804032304306, 1.000000000000000000, 0.9807852804032304306, 1.000000000000000000, 0.9807852804032304306, 1.000000000000000000, 0.9807852804032304306, 1.000000000000000000, 0.9807852804032304306, 1.000000000000000000, 0.9807852804032304306, 1.000000000000000000, 0.9807852804032304306, 1.000000000000000000, 0.9807852804032304306, 1.000000000000000000, 0.9807852804032304306, 1.000000000000000000, 0.9807852804032304306, 1.000000000000000000, 0.9807852804032304306, 1.000000000000000000, 0.9807852804032304306, 1.000000000000000000, 0.9807852804032304306, 1.000000000000000000, 0.9807852804032304306, 1.000000000000000000, 0.9807852804032304306, 1.000000000000000000, 0.9807852804032304306, 1.000000000000000000, 0.9807852804032304306, 1.000000000000000000, 0.9807852804032304306, 1.000000000000000000, 0.9807852804032304306, 1.000000000000000000, 0.9807852804032304306, 1.000000000000000000, 0.9807852804032304306, 1.000000000000000000, 0.9807852804032304306, 1.000000000000000000, 0.9807852804032304306, 1.000000000000000000, 0.9807852804032304306, 1.000000000000000000, 0.9807852804032304306, 1.000000000000000000, 0.9807852804032304306, 1.000000000000000000, 0.9807852804032304306, 1.000000000000000000, 0.9807852804032304306, 1.000000000000000000, 0.9807852804032304306, 1.000000000000000000, 0.9807852804032304306, 1.000000000000000000, 0.9807852804032304306, 1.000000000000000000, 0.9807852804032304306, 1.000000000000000000, 0.9807852804032304306, 1.000000000000000000, 0.9807852804032304306, 1.000000000000000000, 0.9807852804032304306, 1.000000000000000000, 0.9807852804032304306, 1.000000000000000000, 0.9807852804032304306, 1.000000000000000000, 0.9807852804032304306, 1.000000000000000000, 0.9807852804032304306, 1.000000000000000000, 0.9807852804032304306, 1.000000000000000000, 0.9807852804032304306, 1.000000000000000000, 0.9807852804032304306, 1.000000000000000000, 0.9807852804032304306, 1.000000000000000000, 0.9807852804032304306, 1.000000000000000000, 0.9807852804032304306, 1.000000000000000000, 0.9807852804032304306, 1.000000000000000000, 0.9807852804032304306, 1.000000000000000000, 0.9807852804032304306, 1.000000000000000000, 0.9807852804032304306, 1.000000000000000000, 0.9807852804032304306, 1.000000000000000000, 0.9807852804032304306, 1.000000000000000000, 0.9807852804032304306, 1.000000000000000000, 0.9807852804032304306, 1.000000000000000000, 0.9807852804032304306, 1.000000000000000000, 0.9807852804032304306, 1.000000000000000000, 0.9807852804032304306, 1.000000000000000000, 0.9807852804032304306, 1.000000000000000000, 0.9807852804032304306, 1.000000000000000000, 0.9807852804032304306, 1.000000000000000000, 0.9807852804032304306, 1.000000000000000000, 0.9807852804032304306, 1.000000000000000000, 0.9935443096272227326, 0.9914265371698519624),
 ( 1.000000000000000000, 0.9807852804032304306, 1.000000000000000000, 0.9807852804032304306, 1.000000000000000000, 0.9807852804032304306, 1.000000000000000000, 0.9807852804032304306, 1.000000000000000000, 0.9807852804032304306, 1.000000000000000000, 0.9807852804032304306, 1.000000000000000000, 0.9807852804032304306, 1.000000000000000000, 0.9807852804032304306, 1.000000000000000000, 0.9807852804032304306, 1.000000000000000000, 0.9807852804032304306, 1.000000000000000000, 0.9807852804032304306, 1.000000000000000000, 0.9807852804032304306, 1.000000000000000000, 0.9807852804032304306, 1.000000000000000000, 0.9807852804032304306, 1.000000000000000000, 0.9807852804032304306, 1.000000000000000000, 0.9807852804032304306, 1.000000000000000000, 0.9807852804032304306, 1.000000000000000000, 0.9807852804032304306, 1.000000000000000000, 0.9807852804032304306, 1.000000000000000000, 0.9807852804032304306, 1.000000000000000000, 0.9807852804032304306, 1.000000000000000000, 0.9807852804032304306, 1.000000000000000000, 0.9807852804032304306, 1.000000000000000000, 0.9807852804032304306, 1.000000000000000000, 0.9807852804032304306, 1.000000000000000000, 0.9807852804032304306, 1.000000000000000000, 0.9807852804032304306, 1.000000000000000000, 0.9807852804032304306, 1.000000000000000000, 0.9807852804032304306, 1.000000000000000000, 0.9807852804032304306, 1.000000000000000000, 0.9807852804032304306, 1.000000000000000000, 0.9807852804032304306, 1.000000000000000000, 0.9807852804032304306, 1.000000000000000000, 0.9807852804032304306, 1.000000000000000000, 0.9807852804032304306, 1.000000000000000000, 0.9807852804032304306, 1.000000000000000000, 0.9807852804032304306, 1.000000000000000000, 0.9807852804032304306, 1.000000000000000000, 0.9807852804032304306, 1.000000000000000000, 0.9807852804032304306, 1.000000000000000000, 0.9807852804032304306, 1.000000000000000000, 0.9807852804032304306, 1.000000000000000000, 0.9807852804032304306, 1.000000000000000000, 0.9807852804032304306, 1.000000000000000000, 0.9807852804032304306, 1.000000000000000000, 0.9807852804032304306, 1.000000000000000000, 0.9807852804032304306, 1.000000000000000000, 0.9807852804032304306, 1.000000000000000000, 0.9807852804032304306, 1.000000000000000000, 0.9807852804032304306, 1.000000000000000000, 0.9807852804032304306, 1.000000000000000000, 0.9807852804032304306, 1.000000000000000000, 0.9807852804032304306, 1.000000000000000000, 0.9807852804032304306, 1.000000000000000000, 0.9807852804032304306, 1.000000000000000000, 0.9807852804032304306, 1.000000000000000000, 0.9807852804032304306, 1.000000000000000000, 0.9807852804032304306, 1.000000000000000000, 0.9807852804032304306, 1.000000000000000000, 0.9807852804032304306, 1.000000000000000000, 0.9807852804032304306, 1.000000000000000000, 0.9807852804032304306, 1.000000000000000000, 0.9807852804032304306, 1.000000000000000000, 0.9807852804032304306, 1.000000000000000000, 0.9807852804032304306, 1.000000000000000000, 0.9807852804032304306, 1.000000000000000000, 0.9807852804032304306, 1.000000000000000000, 0.9807852804032304306, 1.000000000000000000, 0.9807852804032304306, 1.000000000000000000, 0.9807852804032304306, 1.000000000000000000, 0.9807852804032304306, 1.000000000000000000, 0.9807852804032304306, 1.000000000000000000, 0.9807852804032304306, 1.000000000000000000, 0.9807852804032304306, 1.000000000000000000, 0.9807852804032304306, 1.000000000000000000, 0.9807852804032304306, 1.000000000000000000, 0.9807852804032304306, 1.000000000000000000, 0.9807852804032304306, 1.000000000000000000, 0.9807852804032304306, 1.000000000000000000, 0.9807852804032304306, 1.000000000000000000, 0.9807852804032304306, 1.000000000000000000, 0.9807852804032304306, 1.000000000000000000, 0.9807852804032304306, 1.000000000000000000, 0.9807852804032304306, 1.000000000000000000, 0.9807852804032304306, 1.000000000000000000, 0.9807852804032304306, 1.000000000000000000, 0.9807852804032304306, 1.000000000000000000, 0.9807852804032304306, 1.000000000000000000, 0.9807852804032304306, 1.000000000000000000, 0.9807852804032304306, 1.000000000000000000, 0.9807852804032304306, 1.000000000000000000, 0.9807852804032304306, 1.000000000000000000, 0.9807852804032304306, 1.000000000000000000, 0.9807852804032304306, 1.000000000000000000, 0.9807852804032304306, 1.000000000000000000, 0.9807852804032304306, 1.000000000000000000, 0.9807852804032304306, 1.000000000000000000, 0.9807852804032304306, 1.000000000000000000, 0.9807852804032304306, 1.000000000000000000, 0.9807852804032304306, 1.000000000000000000, 0.9807852804032304306, 1.000000000000000000, 0.9807852804032304306, 1.000000000000000000, 0.9807852804032304306, 1.000000000000000000, 0.9807852804032304306, 1.000000000000000000, 0.9807852804032304306, 1.000000000000000000, 0.9807852804032304306, 1.000000000000000000, 0.9807852804032304306, 1.000000000000000000, 0.9807852804032304306, 1.000000000000000000, 0.9807852804032304306, 1.000000000000000000, 0.9807852804032304306, 1.000000000000000000, 0.9807852804032304306, 1.000000000000000000, 0.9807852804032304306, 1.000000000000000000, 0.9807852804032304306, 1.000000000000000000, 0.9807852804032304306, 1.000000000000000000, 0.9807852804032304306, 1.000000000000000000, 0.9807852804032304306, 1.000000000000000000, 0.9807852804032304306, 1.000000000000000000, 0.9807852804032304306, 1.000000000000000000, 0.9807852804032304306, 1.000000000000000000, 0.9807852804032304306, 1.000000000000000000, 0.9807852804032304306, 1.000000000000000000, 0.9807852804032304306, 1.000000000000000000, 0.9807852804032304306, 1.000000000000000000, 0.9807852804032304306, 1.000000000000000000, 0.9807852804032304306, 1.000000000000000000, 0.9807852804032304306, 1.000000000000000000, 0.9807852804032304306, 1.000000000000000000, 0.9807852804032304306, 1.000000000000000000, 0.9807852804032304306, 1.000000000000000000, 0.9807852804032304306, 1.000000000000000000, 0.9807852804032304306, 1.000000000000000000, 0.9807852804032304306, 1.000000000000000000, 0.9807852804032304306, 1.000000000000000000, 0.9807852804032304306, 1.000000000000000000, 0.9807852804032304306, 1.000000000000000000, 0.9807852804032304306, 1.000000000000000000, 0.9807852804032304306, 1.000000000000000000, 0.9807852804032304306, 1.000000000000000000, 0.9807852804032304306, 1.000000000000000000, 0.9807852804032304306, 1.000000000000000000, 0.9807852804032304306, 1.000000000000000000, 0.9807852804032304306, 1.000000000000000000, 0.9807852804032304306, 1.000000000000000000, 0.9807852804032304306, 1.000000000000000000, 0.9807852804032304306, 1.000000000000000000, 0.9807852804032304306, 1.000000000000000000, 0.9807852804032304306, 1.000000000000000000, 0.9807852804032304306, 1.000000000000000000, 0.9807852804032304306, 1.000000000000000000, 0.9807852804032304306, 1.000000000000000000, 0.9807852804032304306, 1.000000000000000000, 0.9807852804032304306, 1.000000000000000000, 0.9807852804032304306, 1.000000000000000000, 0.9807852804032304306, 1.000000000000000000, 0.9807852804032304306, 1.000000000000000000, 0.9807852804032304306, 1.000000000000000000, 0.9807852804032304306, 1.000000000000000000, 0.9807852804032304306, 1.000000000000000000, 0.9807852804032304306, 1.000000000000000000, 0.9807852804032304306, 1.000000000000000000, 0.9807852804032304306, 1.000000000000000000, 0.9807852804032304306, 1.000000000000000000, 0.9807852804032304306, 1.000000000000000000, 0.9807852804032304306, 1.000000000000000000, 0.9807852804032304306, 1.000000000000000000, 0.9807852804032304306, 1.000000000000000000, 0.9807852804032304306, 1.000000000000000000, 0.9807852804032304306, 1.000000000000000000, 0.9807852804032304306, 1.000000000000000000, 0.9807852804032304306, 1.000000000000000000, 0.9807852804032304306, 1.000000000000000000, 0.9807852804032304306, 1.000000000000000000, 0.9807852804032304306, 1.000000000000000000, 0.9807852804032304306, 1.000000000000000000, 0.9807852804032304306, 1.000000000000000000, 0.9807852804032304306, 1.000000000000000000, 0.9807852804032304306, 1.000000000000000000, 0.9807852804032304306, 1.000000000000000000, 0.9807852804032304306, 1.000000000000000000, 0.9807852804032304306, 1.000000000000000000, 0.9807852804032304306, 1.000000000000000000, 0.9807852804032304306, 1.000000000000000000, 0.9807852804032304306, 1.000000000000000000, 0.9807852804032304306, 1.000000000000000000, 0.9807852804032304306, 1.000000000000000000, 0.9807852804032304306, 1.000000000000000000, 0.9807852804032304306, 1.000000000000000000, 0.9807852804032304306, 1.000000000000000000, 0.9807852804032304306, 1.000000000000000000, 0.9807852804032304306, 1.000000000000000000, 0.9807852804032304306, 1.000000000000000000, 0.9807852804032304306, 1.000000000000000000, 0.9807852804032304306, 1.000000000000000000, 0.9807852804032304306, 1.000000000000000000, 0.9807852804032304306, 1.000000000000000000, 0.9807852804032304306, 1.000000000000000000, 0.9807852804032304306, 1.000000000000000000, 0.9807852804032304306, 1.000000000000000000, 0.9807852804032304306, 1.000000000000000000, 0.9807852804032304306, 1.000000000000000000, 0.9807852804032304306, 1.000000000000000000, 0.9807852804032304306, 1.000000000000000000, 0.9807852804032304306, 1.000000000000000000, 0.9807852804032304306, 1.000000000000000000, 0.9807852804032304306, 1.000000000000000000, 0.9807852804032304306, 1.000000000000000000, 0.9807852804032304306, 1.000000000000000000, 0.9807852804032304306, 1.000000000000000000, 0.9807852804032304306, 1.000000000000000000, 0.9807852804032304306, 1.000000000000000000, 0.9807852804032304306, 1.000000000000000000, 0.9807852804032304306, 1.000000000000000000, 0.9807852804032304306, 1.000000000000000000, 0.9807852804032304306, 1.000000000000000000, 0.9807852804032304306, 1.000000000000000000, 0.9807852804032304306, 1.000000000000000000, 0.9807852804032304306, 1.000000000000000000, 0.9807852804032304306, 1.000000000000000000, 0.9807852804032304306, 1.000000000000000000, 0.9807852804032304306, 1.000000000000000000, 0.9807852804032304306, 1.000000000000000000, 0.9807852804032304306, 1.000000000000000000, 0.9807852804032304306, 1.000000000000000000, 0.9807852804032304306, 1.000000000000000000, 0.9807852804032304306, 1.000000000000000000, 0.9807852804032304306, 1.000000000000000000, 0.9807852804032304306, 1.000000000000000000, 0.9807852804032304306, 1.000000000000000000, 0.9807852804032304306, 1.000000000000000000, 0.9807852804032304306, 1.000000000000000000, 0.9807852804032304306, 1.000000000000000000, 0.9807852804032304306, 1.000000000000000000, 0.9807852804032304306, 1.000000000000000000, 0.9807852804032304306, 1.000000000000000000, 0.9807852804032304306, 1.000000000000000000, 0.9807852804032304306, 1.000000000000000000, 0.9807852804032304306, 1.000000000000000000, 0.9807852804032304306, 1.000000000000000000, 0.9807852804032304306, 1.000000000000000000, 0.9807852804032304306, 1.000000000000000000, 0.9807852804032304306, 1.000000000000000000, 0.9807852804032304306, 1.000000000000000000, 0.9807852804032304306, 1.000000000000000000, 0.9807852804032304306, 1.000000000000000000, 0.9807852804032304306, 1.000000000000000000, 0.9807852804032304306, 1.000000000000000000, 0.9807852804032304306, 1.000000000000000000, 0.9807852804032304306, 1.000000000000000000, 0.9807852804032304306, 1.000000000000000000, 0.9807852804032304306, 1.000000000000000000, 0.9807852804032304306, 1.000000000000000000, 0.9807852804032304306, 1.000000000000000000, 0.9807852804032304306, 1.000000000000000000, 0.9807852804032304306, 1.000000000000000000, 0.9807852804032304306, 1.000000000000000000, 0.9807852804032304306, 1.000000000000000000, 0.9807852804032304306, 1.000000000000000000, 0.9807852804032304306, 1.000000000000000000, 0.9807852804032304306, 1.000000000000000000, 0.9807852804032304306, 1.000000000000000000, 0.9807852804032304306, 1.000000000000000000, 0.9807852804032304306, 1.000000000000000000, 0.9807852804032304306, 1.000000000000000000, 0.9807852804032304306, 1.000000000000000000, 0.9807852804032304306, 1.000000000000000000, 0.9807852804032304306, 1.000000000000000000, 0.9807852804032304306, 1.000000000000000000, 0.9807852804032304306, 1.000000000000000000, 0.9807852804032304306, 1.000000000000000000, 0.9807852804032304306, 1.000000000000000000, 0.9807852804032304306, 1.000000000000000000, 0.9807852804032304306, 1.000000000000000000, 0.9807852804032304306, 1.000000000000000000, 0.9807852804032304306, 1.000000000000000000, 0.9807852804032304306, 1.000000000000000000, 0.9807852804032304306, 1.000000000000000000, 0.9807852804032304306, 1.000000000000000000, 0.9807852804032304306, 1.000000000000000000, 0.9807852804032304306, 1.000000000000000000, 0.9807852804032304306, 1.000000000000000000, 0.9807852804032304306, 1.000000000000000000, 0.9807852804032304306, 1.000000000000000000, 0.9807852804032304306, 1.000000000000000000, 0.9807852804032304306, 1.000000000000000000, 0.9807852804032304306, 1.000000000000000000, 0.9807852804032304306, 1.000000000000000000, 0.9807852804032304306, 1.000000000000000000, 0.9807852804032304306, 1.000000000000000000, 0.9807852804032304306, 1.000000000000000000, 0.9807852804032304306, 1.000000000000000000, 0.9807852804032304306, 1.000000000000000000, 0.9807852804032304306, 1.000000000000000000, 0.9807852804032304306, 1.000000000000000000, 0.9807852804032304306, 1.000000000000000000, 0.9807852804032304306, 1.000000000000000000, 0.9807852804032304306, 1.000000000000000000, 0.9807852804032304306, 1.000000000000000000, 0.9807852804032304306, 1.000000000000000000, 0.9807852804032304306, 1.000000000000000000, 0.9807852804032304306, 1.000000000000000000, 0.9807852804032304306, 1.000000000000000000, 0.9807852804032304306, 1.000000000000000000, 0.9807852804032304306, 1.000000000000000000, 0.9807852804032304306, 1.000000000000000000, 0.9807852804032304306, 1.000000000000000000, 0.9807852804032304306, 1.000000000000000000, 0.9807852804032304306, 1.000000000000000000, 0.9807852804032304306, 1.000000000000000000, 0.9807852804032304306, 1.000000000000000000, 0.9807852804032304306, 1.000000000000000000, 0.9807852804032304306, 1.000000000000000000, 0.9807852804032304306, 1.000000000000000000, 0.9807852804032304306, 1.000000000000000000, 0.9807852804032304306, 1.000000000000000000, 0.9807852804032304306, 1.000000000000000000, 0.9807852804032304306, 1.000000000000000000, 0.9807852804032304306, 1.000000000000000000, 0.9807852804032304306, 1.000000000000000000, 0.9807852804032304306, 1.000000000000000000, 0.9807852804032304306, 1.000000000000000000, 0.9807852804032304306, 1.000000000000000000, 0.9807852804032304306, 1.000000000000000000, 0.9807852804032304306, 1.000000000000000000, 0.9807852804032304306, 1.000000000000000000, 0.9807852804032304306, 1.000000000000000000, 0.9807852804032304306, 1.000000000000000000, 0.9807852804032304306, 1.000000000000000000, 0.9807852804032304306, 1.000000000000000000, 0.9807852804032304306, 1.000000000000000000, 0.9807852804032304306, 1.000000000000000000, 0.9807852804032304306, 1.000000000000000000, 0.9807852804032304306, 1.000000000000000000, 0.9807852804032304306, 1.000000000000000000, 0.9807852804032304306, 1.000000000000000000, 0.9807852804032304306, 1.000000000000000000, 0.9807852804032304306, 1.000000000000000000, 0.9807852804032304306, 1.000000000000000000, 0.9807852804032304306, 1.000000000000000000, 0.9807852804032304306, 1.000000000000000000, 0.9807852804032304306, 1.000000000000000000, 0.9807852804032304306, 1.000000000000000000, 0.9807852804032304306, 1.000000000000000000, 0.9807852804032304306, 1.000000000000000000, 0.9807852804032304306, 1.000000000000000000, 0.9807852804032304306, 1.000000000000000000, 0.9807852804032304306, 1.000000000000000000, 0.9807852804032304306, 1.000000000000000000, 0.9807852804032304306, 1.000000000000000000, 0.9807852804032304306, 1.000000000000000000, 0.9807852804032304306, 1.000000000000000000, 0.9807852804032304306, 1.000000000000000000, 0.9807852804032304306, 1.000000000000000000, 0.9807852804032304306, 1.000000000000000000, 0.9807852804032304306, 1.000000000000000000, 0.9807852804032304306, 1.000000000000000000, 0.9807852804032304306, 1.000000000000000000, 0.9807852804032304306, 1.000000000000000000, 0.9807852804032304306, 1.000000000000000000, 0.9807852804032304306, 1.000000000000000000, 0.9807852804032304306, 1.000000000000000000, 0.9807852804032304306, 1.000000000000000000, 0.9807852804032304306, 1.000000000000000000, 0.9807852804032304306, 1.000000000000000000, 0.9807852804032304306, 1.000000000000000000, 0.9807852804032304306, 1.000000000000000000, 0.9807852804032304306, 1.000000000000000000, 0.9807852804032304306, 1.000000000000000000, 0.9807852804032304306, 1.000000000000000000, 0.9807852804032304306, 1.000000000000000000, 0.9807852804032304306, 1.000000000000000000, 0.9807852804032304306, 1.000000000000000000, 0.9807852804032304306, 1.000000000000000000, 0.9807852804032304306, 1.000000000000000000, 0.9807852804032304306, 1.000000000000000000, 0.9807852804032304306, 1.000000000000000000, 0.9807852804032304306, 1.000000000000000000, 0.9807852804032304306, 1.000000000000000000, 0.9807852804032304306, 1.000000000000000000, 0.9807852804032304306, 1.000000000000000000, 0.9807852804032304306, 1.000000000000000000, 0.9807852804032304306, 1.000000000000000000, 0.9807852804032304306, 1.000000000000000000, 0.9807852804032304306, 1.000000000000000000, 0.9807852804032304306, 1.000000000000000000, 0.9807852804032304306, 1.000000000000000000, 0.9807852804032304306, 1.000000000000000000, 0.9807852804032304306, 1.000000000000000000, 0.9807852804032304306, 1.000000000000000000, 0.9807852804032304306, 1.000000000000000000, 0.9807852804032304306, 1.000000000000000000, 0.9807852804032304306, 1.000000000000000000, 0.9807852804032304306, 1.000000000000000000, 0.9807852804032304306, 1.000000000000000000, 0.9807852804032304306, 1.000000000000000000, 0.9807852804032304306, 1.000000000000000000, 0.9807852804032304306, 1.000000000000000000, 0.9807852804032304306, 1.000000000000000000, 0.9807852804032304306, 1.000000000000000000, 0.9807852804032304306, 1.000000000000000000, 0.9807852804032304306, 1.000000000000000000, 0.9807852804032304306, 1.000000000000000000, 0.9807852804032304306, 1.000000000000000000, 0.9807852804032304306, 1.000000000000000000, 0.9807852804032304306, 1.000000000000000000, 0.9807852804032304306, 1.000000000000000000, 0.9807852804032304306, 1.000000000000000000, 0.9807852804032304306, 1.000000000000000000, 0.9807852804032304306, 1.000000000000000000, 0.9807852804032304306, 1.000000000000000000, 0.9807852804032304306, 1.000000000000000000, 0.9807852804032304306, 1.000000000000000000, 0.9807852804032304306, 1.000000000000000000, 0.9807852804032304306, 1.000000000000000000, 0.9807852804032304306, 1.000000000000000000, 0.9807852804032304306, 1.000000000000000000, 0.9807852804032304306, 1.000000000000000000, 0.9807852804032304306, 1.000000000000000000, 0.9807852804032304306, 1.000000000000000000, 0.9807852804032304306, 1.000000000000000000, 0.9807852804032304306, 1.000000000000000000, 0.9807852804032304306, 1.000000000000000000, 0.9807852804032304306, 1.000000000000000000, 0.9807852804032304306, 1.000000000000000000, 0.9807852804032304306, 1.000000000000000000, 0.9807852804032304306, 1.000000000000000000, 0.9807852804032304306, 1.000000000000000000, 0.9807852804032304306, 1.000000000000000000, 0.9807852804032304306, 1.000000000000000000, 0.9807852804032304306, 1.000000000000000000, 0.9807852804032304306, 1.000000000000000000, 0.9807852804032304306, 1.000000000000000000, 0.9807852804032304306, 1.000000000000000000, 0.9807852804032304306, 1.000000000000000000, 0.9807852804032304306, 1.000000000000000000, 0.9807852804032304306, 1.000000000000000000, 0.9807852804032304306, 1.000000000000000000, 0.9807852804032304306, 1.000000000000000000, 0.9807852804032304306, 1.000000000000000000, 0.9807852804032304306, 1.000000000000000000, 0.9807852804032304306, 1.000000000000000000, 0.9807852804032304306, 1.000000000000000000, 0.9807852804032304306, 1.000000000000000000, 0.9807852804032304306, 1.000000000000000000, 0.9807852804032304306, 1.000000000000000000, 0.9807852804032304306, 1.000000000000000000, 0.9807852804032304306, 1.000000000000000000, 0.9807852804032304306, 1.000000000000000000, 0.9807852804032304306, 1.000000000000000000, 0.9807852804032304306, 1.000000000000000000, 0.9807852804032304306, 1.000000000000000000, 0.9807852804032304306, 1.000000000000000000, 0.9807852804032304306, 1.000000000000000000, 0.9807852804032304306, 1.000000000000000000, 0.9807852804032304306, 1.000000000000000000, 0.9807852804032304306, 1.000000000000000000, 0.9807852804032304306, 1.000000000000000000, 0.9807852804032304306, 1.000000000000000000, 0.9807852804032304306, 1.000000000000000000, 0.9807852804032304306, 1.000000000000000000, 0.9807852804032304306, 1.000000000000000000, 0.9807852804032304306, 1.000000000000000000, 0.9807852804032304306, 1.000000000000000000, 0.9807852804032304306, 1.000000000000000000, 0.9807852804032304306, 1.000000000000000000, 0.9807852804032304306, 1.000000000000000000, 0.9807852804032304306, 1.000000000000000000, 0.9807852804032304306, 1.000000000000000000, 0.9807852804032304306, 1.000000000000000000, 0.9807852804032304306, 1.000000000000000000, 0.9807852804032304306, 1.000000000000000000, 0.9807852804032304306, 1.000000000000000000, 0.9807852804032304306, 1.000000000000000000, 0.9807852804032304306, 1.000000000000000000, 0.9807852804032304306, 1.000000000000000000, 0.9807852804032304306, 1.000000000000000000, 0.9807852804032304306, 1.000000000000000000, 0.9807852804032304306, 1.000000000000000000, 0.9807852804032304306, 1.000000000000000000, 0.9807852804032304306, 1.000000000000000000, 0.9807852804032304306, 1.000000000000000000, 0.9807852804032304306, 1.000000000000000000, 0.9807852804032304306, 1.000000000000000000, 0.9807852804032304306, 1.000000000000000000, 0.9807852804032304306, 1.000000000000000000, 0.9807852804032304306, 1.000000000000000000, 0.9807852804032304306, 1.000000000000000000, 0.9807852804032304306, 1.000000000000000000, 0.9807852804032304306, 1.000000000000000000, 0.9807852804032304306, 1.000000000000000000, 0.9807852804032304306, 1.000000000000000000, 0.9807852804032304306, 1.000000000000000000, 0.9807852804032304306, 1.000000000000000000, 0.9807852804032304306, 1.000000000000000000, 0.9807852804032304306, 1.000000000000000000, 0.9807852804032304306, 1.000000000000000000, 0.9807852804032304306, 1.000000000000000000, 0.9807852804032304306, 1.000000000000000000, 0.9807852804032304306, 1.000000000000000000, 0.9807852804032304306, 1.000000000000000000, 0.9807852804032304306, 1.000000000000000000, 0.9807852804032304306, 1.000000000000000000, 0.9935443096272227326, 0.9914265371698519624) ) ) 
 REPRESENTATION_ITEM ( '' )  SURFACE ( )  );
#12618 = CARTESIAN_POINT ( 'NONE',  ( -45.43829269268869098, 255.0573905683720000, -3.332260488124726194 ) ) ;
#12619 = ORIENTED_EDGE ( 'NONE', *, *, #4848, .T. ) ;
#12620 = ORIENTED_EDGE ( 'NONE', *, *, #6973, .F. ) ;
#12621 = CARTESIAN_POINT ( 'NONE',  ( 6.416697501590670427, 172.9933428177121471, 60.00000000000000000 ) ) ;
#12622 = ORIENTED_EDGE ( 'NONE', *, *, #9889, .F. ) ;
#12623 = CARTESIAN_POINT ( 'NONE',  ( -11.93348319268873325, 460.3698905683720000, -2.051577885510841163E-15 ) ) ;
#12624 = ORIENTED_EDGE ( 'NONE', *, *, #2631, .T. ) ;
#12625 = DIRECTION ( 'NONE',  ( 0.9999562017632421806, 0.000000000000000000, -0.009359196291876339252 ) ) ;
#12626 = CARTESIAN_POINT ( 'NONE',  ( -13.20868407381884779, 239.4948905683720284, -6.410867750099233042 ) ) ;
#12627 = VERTEX_POINT ( 'NONE', #17371 ) ;
#12628 = CARTESIAN_POINT ( 'NONE',  ( -16.84014894278201169, 520.1198905683720568, -11.84573899990672707 ) ) ;
#12629 = DIRECTION ( 'NONE',  ( -0.000000000000000000, -1.000000000000000000, -0.000000000000000000 ) ) ;
#12630 = EDGE_CURVE ( 'NONE', #13370, #1912, #2554, .T. ) ;
#12631 = CARTESIAN_POINT ( 'NONE',  ( -17.35679799567830273, 455.4323905765655809, 16.95518130045146421 ) ) ;
#12632 = CARTESIAN_POINT ( 'NONE',  ( -2.371692252312040949E-15, -5.948846446048902337, 2.696295709017763276 ) ) ;
#12633 = CARTESIAN_POINT ( 'NONE',  ( -8.685887942688802710, 286.6823905765655809, 3.978247347593374172 ) ) ;
#12634 = CARTESIAN_POINT ( 'NONE',  ( -31.15659063867058265, 223.9102039777115749, -18.01685762724678597 ) ) ;
#12635 = CARTESIAN_POINT ( 'NONE',  ( -11.93348319268870661, 230.6823905683720284, -3.332260488124732856 ) ) ;
#12636 = FACE_OUTER_BOUND ( 'NONE', #13636, .T. ) ;
#12637 = CARTESIAN_POINT ( 'NONE',  ( -35.09675569278793716, 235.7448905683720000, 15.47720386886985366 ) ) ;
#12638 = CARTESIAN_POINT ( 'NONE',  ( -14.48388495494899608, 331.3073905683720000, -9.489475012073736337 ) ) ;
#12639 = EDGE_CURVE ( 'NONE', #17724, #264, #13602, .T. ) ;
#12640 = CARTESIAN_POINT ( 'NONE',  ( -49.57497958038186425, 230.5765313837437418, 49.99999999999999289 ) ) ;
#12641 = CARTESIAN_POINT ( 'NONE',  ( -48.68588794268873698, 573.2448905601785327, 0.000000000000000000 ) ) ;
#12642 = CARTESIAN_POINT ( 'NONE',  ( -44.16309181155855867, 305.9948905683720568, 6.410867750099241924 ) ) ;
#12643 = CARTESIAN_POINT ( 'NONE',  ( -44.16309181155856578, 384.4948905683720000, 6.410867750099241924 ) ) ;
#12644 = CARTESIAN_POINT ( 'NONE',  ( -16.84014894278201169, 531.6198905683720568, -11.84573899990672707 ) ) ;
#12645 = CARTESIAN_POINT ( 'NONE',  ( -45.64106924314019409, 396.3073905601785327, -11.32908994701042715 ) ) ;
#12646 = CARTESIAN_POINT ( 'NONE',  ( 105.7989814974898479, 152.5259582928263740, -40.00000000000000000 ) ) ;
#12647 = ORIENTED_EDGE ( 'NONE', *, *, #19479, .F. ) ;
#12648 = ORIENTED_EDGE ( 'NONE', *, *, #19987, .T. ) ;
#12649 = CARTESIAN_POINT ( 'NONE',  ( -13.20868407381887621, 509.7448905683720000, 6.410867750099229490 ) ) ;
#12650 = ORIENTED_EDGE ( 'NONE', *, *, #12612, .F. ) ;
#12651 = CARTESIAN_POINT ( 'NONE',  ( -19.19641293061497578, 301.9323905683720000, -14.20200298773971603 ) ) ;
#12652 = CARTESIAN_POINT ( 'NONE',  ( -11.93348319268871904, 329.1823905683720568, -3.332260488124732856 ) ) ;
#12653 = CARTESIAN_POINT ( 'NONE',  ( -42.82802356641965247, 270.7448905765656377, -14.14213562373094746 ) ) ;
#12654 = CARTESIAN_POINT ( 'NONE',  ( -42.82802356641967378, 500.7448905765656946, -14.14213562373094746 ) ) ;
#12655 = CARTESIAN_POINT ( 'NONE',  ( -32.01814843081343298, 256.0573905683720000, 16.75240474999999307 ) ) ;
#12656 = CARTESIAN_POINT ( 'NONE',  ( 0.000000000000000000, 0.000000000000000000, 0.000000000000000000 ) ) ;
#12657 = CARTESIAN_POINT ( 'NONE',  ( -13.20868407381886378, 399.7448905683720568, 6.410867750099229490 ) ) ;
#12658 = AXIS2_PLACEMENT_3D ( 'NONE', #16364, #21227, #18078 ) ;
#12659 = DIRECTION ( 'NONE',  ( -1.000000000000000000, 0.000000000000000000, 0.000000000000000000 ) ) ;
#12660 = DIRECTION ( 'NONE',  ( 1.000000000000000000, 0.000000000000000000, 0.000000000000000000 ) ) ;
#12661 = EDGE_CURVE ( 'NONE', #2272, #2808, #5357, .T. ) ;
#12662 = CARTESIAN_POINT ( 'NONE',  ( 168.1770832427592666, 610.7448905601785327, 3.512089204514978746 ) ) ;
#12663 = EDGE_CURVE ( 'NONE', #6223, #6933, #8711, .T. ) ;
#12664 = AXIS2_PLACEMENT_3D ( 'NONE', #6237, #4519, #14381 ) ;
#12665 = CARTESIAN_POINT ( 'NONE',  ( -32.01814843081346140, 451.6823905683720568, -16.75240474999999307 ) ) ;
#12666 = ORIENTED_EDGE ( 'NONE', *, *, #17545, .F. ) ;
#12667 = CARTESIAN_POINT ( 'NONE',  ( -48.68588794268871567, 436.9323905601784759, -3.978247347593158345 ) ) ;
#12668 = VERTEX_POINT ( 'NONE', #1053 ) ;
#12669 = ORIENTED_EDGE ( 'NONE', *, *, #18931, .T. ) ;
#12670 = EDGE_LOOP ( 'NONE', ( #4007, #5801, #7781, #6475, #19051 ) ) ;
#12671 = DIRECTION ( 'NONE',  ( -1.191790137725560488E-16, 1.000000000000000000, -0.000000000000000000 ) ) ;
#12672 = CARTESIAN_POINT ( 'NONE',  ( -8.685887942688717445, 331.9323905601784190, 3.978247347593161010 ) ) ;
#12673 = CARTESIAN_POINT ( 'NONE',  ( -38.17536295476245556, 373.8073905683720568, -14.20200298773971426 ) ) ;
#12674 = CIRCLE ( 'NONE', #1988, 50.00000000000000000 ) ;
#12675 = CARTESIAN_POINT ( 'NONE',  ( -13.68588794268873521, 548.2448905601784190, 1.836970198721029983E-15 ) ) ;
#12676 = CARTESIAN_POINT ( 'NONE',  ( -8.685887942688738761, 506.9948905765655240, -2.449293598294705724E-15 ) ) ;
#12677 = CARTESIAN_POINT ( 'NONE',  ( -19.19641293061498644, 387.3073905683720000, 14.20200298773971426 ) ) ;
#12678 = CARTESIAN_POINT ( 'NONE',  ( -42.88789093042841927, 234.4323905683720284, -9.489475012073736337 ) ) ;
#12679 = CARTESIAN_POINT ( 'NONE',  ( -11.93348319268872615, 398.8698905683720000, -2.051577885510841163E-15 ) ) ;
#12680 = AXIS2_PLACEMENT_3D ( 'NONE', #4912, #65, #18105 ) ;
#12681 = CARTESIAN_POINT ( 'NONE',  ( -36.33955658999050797, 313.8698905765656377, 18.47759065022572500 ) ) ;
#12682 = CARTESIAN_POINT ( 'NONE',  ( 35.96497763894178945, 230.5765313837437418, -40.00000000000000000 ) ) ;
#12683 = CARTESIAN_POINT ( 'NONE',  ( -14.48388495494899431, 309.8073905683721136, -9.489475012073734561 ) ) ;
#12684 = CARTESIAN_POINT ( 'NONE',  ( -11.93348319268873325, 460.3698905683720000, -2.051577885510841163E-15 ) ) ;
#12685 = CARTESIAN_POINT ( 'NONE',  ( -21.03221929538692692, 515.1198905765656946, 18.47759065022572500 ) ) ;
#12686 = CARTESIAN_POINT ( 'NONE',  ( -48.68588794268898567, 367.5573905601784759, 3.978247347592529071 ) ) ;
#12687 = CARTESIAN_POINT ( 'NONE',  ( 14.09825962131072785, 303.6587712403113528, 25.00000000000000000 ) ) ;
#12688 = AXIS2_PLACEMENT_3D ( 'NONE', #8467, #8247, #19837 ) ;
#12689 = CARTESIAN_POINT ( 'NONE',  ( -22.27502019258947641, 358.4948905683720000, 15.47720386886985189 ) ) ;
#12690 = CARTESIAN_POINT ( 'NONE',  ( -16.84014894278200458, 497.6198905683720000, 11.84573899990672530 ) ) ;
#12691 = CARTESIAN_POINT ( 'NONE',  ( -24.70764059509556887, 500.0573905601786464, 19.99999999999998934 ) ) ;
#12692 = CARTESIAN_POINT ( 'NONE',  ( -35.09675569278794427, 331.9948905683720000, -15.47720386886985544 ) ) ;
#12693 = AXIS2_PLACEMENT_3D ( 'NONE', #17001, #18604, #8550 ) ;
#12694 = ORIENTED_EDGE ( 'NONE', *, *, #1048, .T. ) ;
#12695 = CARTESIAN_POINT ( 'NONE',  ( -11.73070664223723369, 261.3073905601784759, 11.32908994701042005 ) ) ;
#12696 = PRODUCT_DEFINITION_SHAPE ( 'NONE', 'NONE',  #21401 ) ;
#12697 = VERTEX_POINT ( 'NONE', #4493 ) ;
#12698 = DIRECTION ( 'NONE',  ( 0.4627175328665442677, 0.000000000000000000, 0.8865057725575724579 ) ) ;
#12699 = B_SPLINE_CURVE_WITH_KNOTS ( 'NONE', 3,
 ( #18629, #18954, #7058, #20693, #5866, #593, #10409, #14108, #10300, #13676, #9109, #2106, #2208, #12151, #7160, #13782, #20267, #18842, #16925, #811, #20483, #15515 ),
 .UNSPECIFIED., .F., .F.,
 ( 4, 2, 2, 2, 2, 2, 2, 2, 2, 2, 4 ),
 ( 0.02361608169583586866, 0.02460001686704667984, 0.02509198445265204552, 0.02558395203825741121, 0.02656788720946822238, 0.02755182238067903355, 0.02853575755188984125, 0.02951969272310065243, 0.03001166030870607362, 0.03050362789431149482, 0.03148756306552231987 ),
 .UNSPECIFIED. ) ;
#12700 = CARTESIAN_POINT ( 'NONE',  ( -14.48388495494900852, 431.3073905683720000, -9.489475012073734561 ) ) ;
#12701 = CARTESIAN_POINT ( 'NONE',  ( -14.54375231895777176, 395.7448905765656377, 14.14213562373094568 ) ) ;
#12702 = CARTESIAN_POINT ( 'NONE',  ( 20.42502041961813930, 230.5765313837437418, 60.00000000000000000 ) ) ;
#12703 = CARTESIAN_POINT ( 'NONE',  ( -19.19641293061498999, 437.3073905683720000, 14.20200298773971426 ) ) ;
#12704 = ORIENTED_EDGE ( 'NONE', *, *, #648, .F. ) ;
#12705 = CARTESIAN_POINT ( 'NONE',  ( -19.19641293061499354, 460.4323905683721136, -14.20200298773971603 ) ) ;
#12706 = DIRECTION ( 'NONE',  ( 0.000000000000000000, 0.000000000000000000, 1.000000000000000000 ) ) ;
#12707 = CARTESIAN_POINT ( 'NONE',  ( -48.68588794268871567, 417.2448905601784759, 0.000000000000000000 ) ) ;
#12708 = CARTESIAN_POINT ( 'NONE',  ( -45.64106924314019409, 392.9323905765656377, 11.32908994701042715 ) ) ;
#12709 = CARTESIAN_POINT ( 'NONE',  ( -32.66413529028186247, 279.8073905765656377, -19.99999999999999289 ) ) ;
#12710 = DIRECTION ( 'NONE',  ( 1.000000000000000000, 0.000000000000000000, 0.000000000000000000 ) ) ;
#12711 = CYLINDRICAL_SURFACE ( 'NONE', #13256, 5.000000000000001776 ) ;
#12712 = CARTESIAN_POINT ( 'NONE',  ( 72.94945500224395118, 285.0140030772282103, -40.00000000000000000 ) ) ;
#12713 = PLANE ( 'NONE',  #6442 ) ;
#12714 = CARTESIAN_POINT ( 'NONE',  ( 158.8141120573112630, 575.7448905601785327, 0.000000000000000000 ) ) ;
#12715 = EDGE_CURVE ( 'NONE', #1587, #6189, #16775, .T. ) ;
#12716 = CARTESIAN_POINT ( 'NONE',  ( -36.66917619319848853, 223.9102039777117170, 18.22452296251983483 ) ) ;
#12717 = CARTESIAN_POINT ( 'NONE',  ( -36.33955658999050087, 239.1198905601784475, 18.47759065022572500 ) ) ;
#12718 = CARTESIAN_POINT ( 'NONE',  ( -14.54375231895777709, 450.9948905601784759, 14.14213562373094568 ) ) ;
#12719 = CARTESIAN_POINT ( 'NONE',  ( -44.16309181155857999, 424.7448905683720000, -6.410867750099231266 ) ) ;
#12720 = CARTESIAN_POINT ( 'NONE',  ( -14.54375231895777176, 383.4948905601784759, -14.14213562373094746 ) ) ;
#12721 = CARTESIAN_POINT ( 'NONE',  ( -25.35362745456396638, 248.1823905683720284, 16.75240474999998952 ) ) ;
#12722 = ORIENTED_EDGE ( 'NONE', *, *, #15553, .T. ) ;
#12723 = DIRECTION ( 'NONE',  ( 0.000000000000000000, 0.000000000000000000, 1.000000000000000000 ) ) ;
#12724 = ORIENTED_EDGE ( 'NONE', *, *, #8275, .F. ) ;
#12725 = CARTESIAN_POINT ( 'NONE',  ( -44.16309181155857999, 455.9948905683720000, 6.410867750099241924 ) ) ;
#12726 = CARTESIAN_POINT ( 'NONE',  ( -36.33955658999050087, 223.8698905765656377, 18.47759065022572500 ) ) ;
#12727 = ORIENTED_EDGE ( 'NONE', *, *, #3797, .T. ) ;
#12728 = FACE_OUTER_BOUND ( 'NONE', #6478, .T. ) ;
#12729 = ORIENTED_EDGE ( 'NONE', *, *, #15335, .F. ) ;
#12730 = CARTESIAN_POINT ( 'NONE',  ( -38.17536295476247687, 532.3073905683719431, -14.20200298773971426 ) ) ;
#12731 = DIRECTION ( 'NONE',  ( 0.000000000000000000, 0.000000000000000000, -1.000000000000000000 ) ) ;
#12732 = EDGE_CURVE ( 'NONE', #17801, #9678, #2982, .T. ) ;
#12733 = CARTESIAN_POINT ( 'NONE',  ( -10.20829729246299777, 456.3698905765656377, 7.653668647301790529 ) ) ;
#12734 = LINE ( 'NONE', #19325, #15169 ) ;
#12735 = CARTESIAN_POINT ( 'NONE',  ( -28.68588794268874054, 573.2448905601785327, 0.000000000000000000 ) ) ;
#12736 = CARTESIAN_POINT ( 'NONE',  ( 0.05533025579362575719, -4.993776679985864497, -4.350525068611871049 ) ) ;
#12737 = CARTESIAN_POINT ( 'NONE',  ( -44.16309181155855157, 225.9948905683720284, 6.410867750099241924 ) ) ;
#12738 = CARTESIAN_POINT ( 'NONE',  ( -29.56664704377478969, 223.9102039777116886, 20.04572207461867706 ) ) ;
#12739 = CARTESIAN_POINT ( 'NONE',  ( -14.48388495494898187, 227.9323905683720000, 9.489475012073732785 ) ) ;
#12740 =( BOUNDED_CURVE ( )  B_SPLINE_CURVE ( 2, ( #2161, #3356, #10042, #6798, #1853, #20114, #15366, #8422, #14935, #11676, #16981, #13310, #8527, #10250, #13631, #8744, #11779 ),
 .UNSPECIFIED., .F., .T. ) 
 B_SPLINE_CURVE_WITH_KNOTS ( ( 3, 2, 2, 2, 2, 2, 2, 2, 3 ),
 ( 0.5937500000000002220, 0.5957031250000002220, 0.5976562500000002220, 0.5996093750000002220, 0.6015625000000002220, 0.6035156250000002220, 0.6054687500000002220, 0.6074218750000002220, 0.6093750000000002220 ),
 .UNSPECIFIED. ) 
 CURVE ( )  GEOMETRIC_REPRESENTATION_ITEM ( )  RATIONAL_B_SPLINE_CURVE ( ( 0.9999999999999977796, 0.9807852804032326510, 1.000000000000000000, 0.9807852804032304306, 1.000000000000000000, 0.9807852804032304306, 1.000000000000000000, 0.9807852804032304306, 1.000000000000000000, 0.9807852804032304306, 1.000000000000000000, 0.9807852804032304306, 1.000000000000000000, 0.9807852804032304306, 1.000000000000000000, 0.9807852804032282101, 1.000000000000002220 ) ) 
 REPRESENTATION_ITEM ( '' )  );
#12741 = CARTESIAN_POINT ( 'NONE',  ( -42.88789093042842637, 324.4323905683719431, -9.489475012073736337 ) ) ;
#12742 = PLANE ( 'NONE',  #17494 ) ;
#12743 = CARTESIAN_POINT ( 'NONE',  ( -47.16347859291444422, 377.8698905601784190, 7.653668647301805628 ) ) ;
#12744 = CARTESIAN_POINT ( 'NONE',  ( -32.01814843081344009, 307.5573905683719431, 16.75240474999999307 ) ) ;
#12745 = VECTOR ( 'NONE', #16598, 1000.000000000000000 ) ;
#12746 = EDGE_CURVE ( 'NONE', #10157, #19472, #7511, .T. ) ;
#12747 = CARTESIAN_POINT ( 'NONE',  ( -28.68588794268871922, 391.3698905683720000, -16.75240474999999307 ) ) ;
#12748 = CARTESIAN_POINT ( 'NONE',  ( -13.20868407381887977, 529.7448905683720568, 6.410867750099229490 ) ) ;
#12749 = CARTESIAN_POINT ( 'NONE',  ( -40.01497788969913927, 375.6823905601784759, -16.95518130045146421 ) ) ;
#12750 = VECTOR ( 'NONE', #17022, 1000.000000000000000 ) ;
#12751 = CARTESIAN_POINT ( 'NONE',  ( -32.66413529028185536, 229.8073905765656377, -19.99999999999999289 ) ) ;
#12752 = ORIENTED_EDGE ( 'NONE', *, *, #9399, .T. ) ;
#12753 = EDGE_LOOP ( 'NONE', ( #1961, #18991, #16240, #8873 ) ) ;
#12754 = CARTESIAN_POINT ( 'NONE',  ( -11.93348319268873681, 490.0573905683720568, 3.332260488124728415 ) ) ;
#12755 = LINE ( 'NONE', #9285, #16302 ) ;
#12756 = ORIENTED_EDGE ( 'NONE', *, *, #17290, .F. ) ;
#12757 = EDGE_CURVE ( 'NONE', #15706, #2560, #16287, .T. ) ;
#12758 = CARTESIAN_POINT ( 'NONE',  ( -32.01814843081344009, 283.1823905683720000, -16.75240474999999307 ) ) ;
#12759 = CARTESIAN_POINT ( 'NONE',  ( -25.35362745456397704, 326.6823905683720568, 16.75240474999998952 ) ) ;
#12760 = CARTESIAN_POINT ( 'NONE',  ( -24.70764059509555111, 269.1823905765655809, -19.99999999999999289 ) ) ;
#12761 = CARTESIAN_POINT ( 'NONE',  ( 3.458603197740078627, 303.6587712403113528, 33.59072564020503648 ) ) ;
#12762 = CARTESIAN_POINT ( 'NONE',  ( -38.17536295476243424, 235.4323905683720284, 14.20200298773971781 ) ) ;
#12763 = CARTESIAN_POINT ( 'NONE',  ( -43.68588794268869435, 223.9102039777116602, 0.000000000000000000 ) ) ;
#12764 = CARTESIAN_POINT ( 'NONE',  ( -42.88789093042843348, 384.4323905683720000, -9.489475012073736337 ) ) ;
#12765 = CIRCLE ( 'NONE', #7213, 10.00000000000000533 ) ;
#12766 = CARTESIAN_POINT ( 'NONE',  ( -42.88695301665256920, 203.8419814082757568, 4.830353110044838694 ) ) ;
#12767 = PLANE ( 'NONE',  #17646 ) ;
#12768 = FACE_OUTER_BOUND ( 'NONE', #1414, .T. ) ;
#12769 = CARTESIAN_POINT ( 'NONE',  ( -42.88789093042844058, 444.8073905683720568, 9.489475012073736337 ) ) ;
#12770 = LINE ( 'NONE', #21303, #12273 ) ;
#12771 = ORIENTED_EDGE ( 'NONE', *, *, #250, .F. ) ;
#12772 = CARTESIAN_POINT ( 'NONE',  ( -24.70764059509557242, 444.4323905601784759, -19.99999999999999289 ) ) ;
#12773 = VERTEX_POINT ( 'NONE', #7726 ) ;
#12774 = VERTEX_POINT ( 'NONE', #16073 ) ;
#12775 = ORIENTED_EDGE ( 'NONE', *, *, #11596, .T. ) ;
#12776 = CARTESIAN_POINT ( 'NONE',  ( -8.685887942688722774, 356.9948905765655809, -2.449293598294705724E-15 ) ) ;
#12777 = CARTESIAN_POINT ( 'NONE',  ( -36.33955658999050797, 335.3698905601784759, -18.47759065022572855 ) ) ;
#12778 = CARTESIAN_POINT ( 'NONE',  ( -44.75779996082702894, 223.9102039777117170, -4.771598740727748478 ) ) ;
#12779 = CARTESIAN_POINT ( 'NONE',  ( -32.01814843081344719, 373.1823905683720568, -16.75240474999999307 ) ) ;
#12780 = CYLINDRICAL_SURFACE ( 'NONE', #3824, 28.29169339157297358 ) ;
#12781 = CARTESIAN_POINT ( 'NONE',  ( -10.20829729246300310, 497.6198905765656377, -7.653668647301794969 ) ) ;
#12782 = CARTESIAN_POINT ( 'NONE',  ( -11.93348319268872437, 388.8698905683720000, -2.051577885510841163E-15 ) ) ;
#12783 = DIRECTION ( 'NONE',  ( 1.000000000000000000, -0.000000000000000000, 0.000000000000000000 ) ) ;
#12784 = EDGE_CURVE ( 'NONE', #14197, #7633, #10865, .T. ) ;
#12785 = CARTESIAN_POINT ( 'NONE',  ( -19.19641293061498644, 400.4323905683720568, -14.20200298773971603 ) ) ;
#12786 = CARTESIAN_POINT ( 'NONE',  ( -32.66413529028186957, 319.8073905765655809, -19.99999999999999289 ) ) ;
#12787 = CARTESIAN_POINT ( 'NONE',  ( -21.03221929538693047, 424.1198905601784759, -18.47759065022572855 ) ) ;
#12788 = CARTESIAN_POINT ( 'NONE',  ( -19.19641293061497223, 287.3073905683720000, 14.20200298773971426 ) ) ;
#12789 = CARTESIAN_POINT ( 'NONE',  ( -13.20868407381887266, 460.9948905683720000, -6.410867750099233042 ) ) ;
#12790 = LINE ( 'NONE', #5753, #5761 ) ;
#12791 = DIRECTION ( 'NONE',  ( -0.000000000000000000, 0.5000000000000012212, 0.8660254037844380415 ) ) ;
#12792 = DIRECTION ( 'NONE',  ( 0.000000000000000000, 0.000000000000000000, -1.000000000000000000 ) ) ;
#12793 = EDGE_CURVE ( 'NONE', #1107, #11848, #54, .T. ) ;
#12794 = AXIS2_PLACEMENT_3D ( 'NONE', #808, #2419, #696 ) ;
#12795 = CARTESIAN_POINT ( 'NONE',  ( -25.35362745456399125, 372.5573905683720568, -16.75240474999999307 ) ) ;
#12796 = CARTESIAN_POINT ( 'NONE',  ( -32.01814843081346851, 511.6823905683720000, -16.75240474999999307 ) ) ;
#12797 = EDGE_CURVE ( 'NONE', #2613, #5272, #4333, .T. ) ;
#12798 = CARTESIAN_POINT ( 'NONE',  ( -21.03221929538694113, 504.1198905601784759, -18.47759065022572855 ) ) ;
#12799 = CARTESIAN_POINT ( 'NONE',  ( -19.19641293061498288, 330.4323905683720000, -14.20200298773971603 ) ) ;
#12800 = EDGE_CURVE ( 'NONE', #5272, #15878, #21358, .T. ) ;
#12801 = EDGE_LOOP ( 'NONE', ( #20388, #1838 ) ) ;
#12802 = DIRECTION ( 'NONE',  ( 1.000000000000000000, 0.000000000000000000, 0.000000000000000000 ) ) ;
#12803 = VERTEX_POINT ( 'NONE', #16292 ) ;
#12804 = DIRECTION ( 'NONE',  ( 0.000000000000000000, -1.000000000000000000, 0.000000000000000000 ) ) ;
#12805 = CARTESIAN_POINT ( 'NONE',  ( -11.93348319268872970, 430.6823905683721136, -3.332260488124732856 ) ) ;
#12806 = CARTESIAN_POINT ( 'NONE',  ( -10.20829729246297291, 236.3698905765656093, 7.653668647301790529 ) ) ;
#12807 = CYLINDRICAL_SURFACE ( 'NONE', #11430, 19.99999999999999645 ) ;
#12808 = CARTESIAN_POINT ( 'NONE',  ( -32.01814843081345430, 436.0573905683720568, 16.75240474999999307 ) ) ;
#12809 = ORIENTED_EDGE ( 'NONE', *, *, #4721, .T. ) ;
#12810 = VECTOR ( 'NONE', #3100, 1000.000000000000000 ) ;
#12811 = CARTESIAN_POINT ( 'NONE',  ( -45.43829269268872650, 473.5573905683720568, -3.332260488124726638 ) ) ;
#12812 = CARTESIAN_POINT ( 'NONE',  ( -162.2727221670389781, 36.20386280891152353, 0.000000000000000000 ) ) ;
#12813 = CARTESIAN_POINT ( 'NONE',  ( -42.82802356641966668, 415.9948905601785327, -14.14213562373094746 ) ) ;
#12814 = EDGE_CURVE ( 'NONE', #11997, #12017, #19622, .T. ) ;
#12815 = CARTESIAN_POINT ( 'NONE',  ( -36.33955658999051508, 383.8698905765656377, 18.47759065022572500 ) ) ;
#12816 = DIRECTION ( 'NONE',  ( 0.000000000000000000, 1.000000000000000000, 0.000000000000000000 ) ) ;
#12817 = CARTESIAN_POINT ( 'NONE',  ( -36.33955658999050797, 370.1198905765656377, -18.47759065022572855 ) ) ;
#12818 = DIRECTION ( 'NONE',  ( 0.000000000000000000, -0.5000000000000009992, 0.8660254037844381525 ) ) ;
#12819 = CARTESIAN_POINT ( 'NONE',  ( -42.82802356641964536, 253.2448905765656377, 14.14213562373094923 ) ) ;
#12820 = MECHANICAL_DESIGN_GEOMETRIC_PRESENTATION_REPRESENTATION (  '', ( #13177 ), #3488 ) ;
#12821 = CARTESIAN_POINT ( 'NONE',  ( 10.41669750159067220, 172.9933428177121471, 50.00000000000000000 ) ) ;
#12822 = AXIS2_PLACEMENT_3D ( 'NONE', #9405, #14406, #6153 ) ;
#12823 = LINE ( 'NONE', #4696, #66 ) ;
#12824 = CARTESIAN_POINT ( 'NONE',  ( -14.54375231895776821, 343.4948905601785327, -14.14213562373094746 ) ) ;
#12825 = CARTESIAN_POINT ( 'NONE',  ( -45.43829269268871229, 425.0573905683720568, -3.332260488124726194 ) ) ;
#12826 = DIRECTION ( 'NONE',  ( 0.000000000000000000, -1.000000000000000000, 0.000000000000000000 ) ) ;
#12827 = CARTESIAN_POINT ( 'NONE',  ( -11.93348319268870839, 240.6823905683720284, -3.332260488124732856 ) ) ;
#12828 = ORIENTED_EDGE ( 'NONE', *, *, #16551, .F. ) ;
#12829 = VERTEX_POINT ( 'NONE', #13142 ) ;
#12830 = CARTESIAN_POINT ( 'NONE',  ( -42.82802356641966668, 423.2448905765656377, 14.14213562373094923 ) ) ;
#12831 = VERTEX_POINT ( 'NONE', #4800 ) ;
#12832 = CARTESIAN_POINT ( 'NONE',  ( -22.27502019258949773, 462.2448905683720568, -15.47720386886985544 ) ) ;
#12833 = CARTESIAN_POINT ( 'NONE',  ( -47.16347859291443001, 222.6198905765656093, 7.653668647301805628 ) ) ;
#12834 = CIRCLE ( 'NONE', #8323, 20.00000000000000000 ) ;
#12835 = ORIENTED_EDGE ( 'NONE', *, *, #522, .T. ) ;
#12836 = CARTESIAN_POINT ( 'NONE',  ( -42.83993802355417557, 205.8067832142904479, 4.966639429937474759 ) ) ;
#12837 = CARTESIAN_POINT ( 'NONE',  ( -22.27502019258950483, 532.2448905683720568, -15.47720386886985544 ) ) ;
#12838 = VERTEX_POINT ( 'NONE', #1682 ) ;
#12839 = CARTESIAN_POINT ( 'NONE',  ( -44.16309181155858710, 524.4948905683719431, 6.410867750099241924 ) ) ;
#12840 = DIRECTION ( 'NONE',  ( 0.000000000000000000, 1.000000000000000000, 0.000000000000000000 ) ) ;
#12841 = CARTESIAN_POINT ( 'NONE',  ( -24.70764059509556176, 434.8073905765656377, 19.99999999999998934 ) ) ;
#12842 = CARTESIAN_POINT ( 'NONE',  ( -28.68588794268871212, 349.7448905601784759, 19.99999999999999289 ) ) ;
#12843 = CARTESIAN_POINT ( 'NONE',  ( -48.68588794268872277, 451.9948905765656377, 0.000000000000000000 ) ) ;
#12844 = CARTESIAN_POINT ( 'NONE',  ( -36.33955658999049376, 240.1198905765656377, -18.47759065022572855 ) ) ;
#12845 = DIRECTION ( 'NONE',  ( 1.191790137725560488E-16, -1.000000000000000000, 0.000000000000000000 ) ) ;
#12846 = PRESENTATION_STYLE_ASSIGNMENT (( #11104 ) ) ;
#12847 = CARTESIAN_POINT ( 'NONE',  ( -8.685887942688726326, 396.9948905765656377, -2.449293598294705724E-15 ) ) ;
#12848 = CARTESIAN_POINT ( 'NONE',  ( -45.43829269268869808, 325.0573905683719431, -3.332260488124726194 ) ) ;
#12849 = CARTESIAN_POINT ( 'NONE',  ( -48.68588794268871567, 447.2448905601785327, 0.000000000000000000 ) ) ;
#12850 = DIRECTION ( 'NONE',  ( 0.000000000000000000, 0.000000000000000000, 1.000000000000000000 ) ) ;
#12851 = VECTOR ( 'NONE', #14813, 1000.000000000000000 ) ;
#12852 = PRESENTATION_LAYER_ASSIGNMENT (  '', '', ( #4219 ) ) ;
#12853 = CARTESIAN_POINT ( 'NONE',  ( -11.93348319268871549, 300.6823905683720568, -3.332260488124732856 ) ) ;
#12854 = EDGE_CURVE ( 'NONE', #15132, #4208, #2260, .T. ) ;
#12855 = CARTESIAN_POINT ( 'NONE',  ( -44.16309181155856578, 354.4948905683720000, 6.410867750099241924 ) ) ;
#12856 = CARTESIAN_POINT ( 'NONE',  ( -44.16309181155859420, 524.7448905683720568, -6.410867750099231266 ) ) ;
#12857 = CARTESIAN_POINT ( 'NONE',  ( -17.35679799567829917, 363.8073905601784759, -16.95518130045146421 ) ) ;
#12858 = CARTESIAN_POINT ( 'NONE',  ( 4.700000000000000178, 3.752776749732560368, -6.499999999999999112 ) ) ;
#12859 = ORIENTED_EDGE ( 'NONE', *, *, #5038, .T. ) ;
#12860 = CARTESIAN_POINT ( 'NONE',  ( -40.53162694259545162, 494.1198905683720000, -11.84573899990672707 ) ) ;
#12861 = FACE_OUTER_BOUND ( 'NONE', #7089, .T. ) ;
#12862 = CARTESIAN_POINT ( 'NONE',  ( -42.88789093042842637, 284.8073905683720568, 9.489475012073736337 ) ) ;
#12863 = ORIENTED_EDGE ( 'NONE', *, *, #577, .T. ) ;
#12864 = CARTESIAN_POINT ( 'NONE',  ( -13.20868407381885135, 280.9948905683720000, -6.410867750099233042 ) ) ;
#12865 = CARTESIAN_POINT ( 'NONE',  ( -35.09675569278794427, 325.7448905683720000, 15.47720386886985366 ) ) ;
#12866 = VECTOR ( 'NONE', #3775, 1000.000000000000000 ) ;
#12867 = EDGE_CURVE ( 'NONE', #10520, #9177, #6416, .T. ) ;
#12868 = CARTESIAN_POINT ( 'NONE',  ( -17.35679799567827786, 255.4323905765656662, 16.95518130045146421 ) ) ;
#12869 = CARTESIAN_POINT ( 'NONE',  ( 2.416697501590669095, 172.9933428177121471, 45.00000000000000000 ) ) ;
#12870 = CARTESIAN_POINT ( 'NONE',  ( -44.16309181155855157, 224.4948905683720284, 6.410867750099241924 ) ) ;
#12871 = DIRECTION ( 'NONE',  ( -1.000000000000000000, 0.000000000000000000, 0.000000000000000000 ) ) ;
#12872 = CARTESIAN_POINT ( 'NONE',  ( -44.16309181155856578, 385.9948905683720568, 6.410867750099241924 ) ) ;
#12873 = CARTESIAN_POINT ( 'NONE',  ( -42.82802356641964536, 205.1437886375728965, 5.000000000000001776 ) ) ;
#12874 = LINE ( 'NONE', #10811, #742 ) ;
#12875 = PRODUCT_DEFINITION_SHAPE ( 'NONE', 'NONE',  #324 ) ;
#12876 = CIRCLE ( 'NONE', #13582, 20.00000000000000355 ) ;
#12877 = LINE ( 'NONE', #17941, #17386 ) ;
#12878 = EDGE_CURVE ( 'NONE', #7385, #14679, #10545, .T. ) ;
#12879 = EDGE_CURVE ( 'NONE', #5562, #14726, #18843, .T. ) ;
#12880 = CARTESIAN_POINT ( 'NONE',  ( -22.27502019258949773, 440.7448905683720000, -15.47720386886985544 ) ) ;
#12881 = CYLINDRICAL_SURFACE ( 'NONE', #17749, 4.000000000000001776 ) ;
#12882 = ORIENTED_EDGE ( 'NONE', *, *, #6167, .T. ) ;
#12883 = CARTESIAN_POINT ( 'NONE',  ( -40.01497788969914637, 425.6823905601784759, -16.95518130045146421 ) ) ;
#12884 = ORIENTED_EDGE ( 'NONE', *, *, #16371, .T. ) ;
#12885 = ORIENTED_EDGE ( 'NONE', *, *, #11201, .T. ) ;
#12886 = ORIENTED_EDGE ( 'NONE', *, *, #5509, .F. ) ;
#12887 = CARTESIAN_POINT ( 'NONE',  ( -10.20829729246298534, 356.3698905765655809, 7.653668647301790529 ) ) ;
#12888 = CARTESIAN_POINT ( 'NONE',  ( -36.33955658999050797, 319.1198905601784759, 18.47759065022572500 ) ) ;
#12889 = PLANE ( 'NONE',  #1795 ) ;
#12890 = CARTESIAN_POINT ( 'NONE',  ( -19.19641293061497933, 341.9323905683721136, -14.20200298773971603 ) ) ;
#12891 = CARTESIAN_POINT ( 'NONE',  ( -42.82802356641968089, 503.2448905765656377, 14.14213562373094923 ) ) ;
#12892 = CARTESIAN_POINT ( 'NONE',  ( -11.93348319268872437, 389.1823905683721136, -3.332260488124732856 ) ) ;
#12893 = FACE_OUTER_BOUND ( 'NONE', #21205, .T. ) ;
#12894 = VECTOR ( 'NONE', #21299, 1000.000000000000000 ) ;
#12895 = CARTESIAN_POINT ( 'NONE',  ( -38.17536295476244845, 385.4323905683720568, 14.20200298773971781 ) ) ;
#12896 = CARTESIAN_POINT ( 'NONE',  ( -10.20829729246298001, 317.6198905765655809, -7.653668647301794969 ) ) ;
#12897 = CARTESIAN_POINT ( 'NONE',  ( -46.31968306282883674, 213.9102039777116602, -33.59072564020502938 ) ) ;
#12898 = CARTESIAN_POINT ( 'NONE',  ( -40.53162694259543031, 292.6198905683720000, -11.84573899990672707 ) ) ;
#12899 = CARTESIAN_POINT ( 'NONE',  ( -35.09675569278795848, 447.2448905683720000, 15.47720386886985366 ) ) ;
#12900 = B_SPLINE_CURVE_WITH_KNOTS ( 'NONE', 3,
 ( #20400, #18766, #12389, #17057, #20296, #5466, #2240, #4164 ),
 .UNSPECIFIED., .F., .F.,
 ( 4, 2, 2, 4 ),
 ( 0.003797433802554464090, 0.004743183970586256973, 0.005688934138618050723, 0.007580434474681636489 ),
 .UNSPECIFIED. ) ;
#12901 = DIRECTION ( 'NONE',  ( 0.000000000000000000, 1.000000000000000000, 0.000000000000000000 ) ) ;
#12902 = DIRECTION ( 'NONE',  ( 0.000000000000000000, 0.000000000000000000, -1.000000000000000000 ) ) ;
#12903 = CARTESIAN_POINT ( 'NONE',  ( -28.68588794268874054, 573.2448905601785327, 0.000000000000000000 ) ) ;
#12904 = CARTESIAN_POINT ( 'NONE',  ( -13.20868407381885845, 350.9948905683720000, -6.410867750099233042 ) ) ;
#12905 = CARTESIAN_POINT ( 'NONE',  ( -11.93348319268873858, 508.8698905683719431, -2.051577885510841163E-15 ) ) ;
#12906 = AXIS2_PLACEMENT_3D ( 'NONE', #4880, #18072, #11695 ) ;
#12907 = CARTESIAN_POINT ( 'NONE',  ( -11.73070664223726567, 493.1823905601785327, -11.32908994701042715 ) ) ;
#12908 = CARTESIAN_POINT ( 'NONE',  ( -16.84014894278198327, 317.6198905683720568, 11.84573899990672530 ) ) ;
#12909 = ORIENTED_EDGE ( 'NONE', *, *, #2617, .F. ) ;
#12910 = CARTESIAN_POINT ( 'NONE',  ( -40.01497788969911795, 258.8073905601784190, 16.95518130045146776 ) ) ;
#12911 = ORIENTED_EDGE ( 'NONE', *, *, #13058, .T. ) ;
#12912 = DIRECTION ( 'NONE',  ( 0.3090169943749472847, -0.000000000000000000, -0.9510565162951536422 ) ) ;
#12913 = CARTESIAN_POINT ( 'NONE',  ( -44.16309181155857289, 405.9948905683720568, 6.410867750099241924 ) ) ;
#12914 = CARTESIAN_POINT ( 'NONE',  ( -11.73070664223723192, 236.0573905765656093, 11.32908994701042005 ) ) ;
#12915 = CARTESIAN_POINT ( 'NONE',  ( 0.000000000000000000, -5.629165124598843661, 3.250000000000012879 ) ) ;
#12916 = CARTESIAN_POINT ( 'NONE',  ( -16.84014894278199748, 447.6198905683720568, 11.84573899990672530 ) ) ;
#12917 = ORIENTED_EDGE ( 'NONE', *, *, #14924, .T. ) ;
#12918 = CARTESIAN_POINT ( 'NONE',  ( -32.01814843081345430, 456.0573905683720000, 16.75240474999999307 ) ) ;
#12919 = CARTESIAN_POINT ( 'NONE',  ( 6.416697501590665986, 217.7548513357007778, -72.61850154709787830 ) ) ;
#12920 = CARTESIAN_POINT ( 'NONE',  ( 28.16023193154655502, 323.8848358243226357, -40.00000000000000000 ) ) ;
#12921 = CARTESIAN_POINT ( 'NONE',  ( -28.68588794268871922, 389.4948905765656377, -19.99999999999999289 ) ) ;
#12922 = CARTESIAN_POINT ( 'NONE',  ( -28.24026808052491688, 46.95427799011174841, 49.59944287259298790 ) ) ;
#12923 = DIRECTION ( 'NONE',  ( -0.000000000000000000, -1.000000000000000000, -0.000000000000000000 ) ) ;
#12924 = DIRECTION ( 'NONE',  ( 0.4627175328665442677, 0.000000000000000000, -0.8865057725575724579 ) ) ;
#12925 = CARTESIAN_POINT ( 'NONE',  ( 3.458603197740078627, 326.0737056351150613, 33.59072564020503648 ) ) ;
#12926 = EDGE_CURVE ( 'NONE', #16401, #5562, #13783, .T. ) ;
#12927 = AXIS2_PLACEMENT_3D ( 'NONE', #17193, #2587, #8845 ) ;
#12928 = CARTESIAN_POINT ( 'NONE',  ( -11.93348319268873858, 500.0573905683720568, 3.332260488124728415 ) ) ;
#12929 = DIRECTION ( 'NONE',  ( 0.000000000000000000, -1.000000000000000000, 0.000000000000000000 ) ) ;
#12930 = CARTESIAN_POINT ( 'NONE',  ( -48.68588794268869435, 257.2448905601784759, 0.000000000000000000 ) ) ;
#12931 = CARTESIAN_POINT ( 'NONE',  ( -8.685887942688818697, 421.9323905601785327, 3.978247347593374172 ) ) ;
#12932 =( BOUNDED_CURVE ( )  B_SPLINE_CURVE ( 2, ( #3850, #18875, #15866, #5789, #6005, #7620, #8821, #7514, #10544, #13926, #13813, #2243, #18769, #3957, #17473, #7300, #17166 ),
 .UNSPECIFIED., .F., .T. ) 
 B_SPLINE_CURVE_WITH_KNOTS ( ( 3, 2, 2, 2, 2, 2, 2, 2, 3 ),
 ( 0.5156250000000002220, 0.5175781250000002220, 0.5195312500000002220, 0.5214843750000002220, 0.5234375000000002220, 0.5253906250000003331, 0.5273437500000003331, 0.5292968750000003331, 0.5312500000000003331 ),
 .UNSPECIFIED. ) 
 CURVE ( )  GEOMETRIC_REPRESENTATION_ITEM ( )  RATIONAL_B_SPLINE_CURVE ( ( 0.9999999999999977796, 0.9807852804032326510, 1.000000000000000000, 0.9807852804032304306, 1.000000000000000000, 0.9807852804032304306, 1.000000000000000000, 0.9807852804032304306, 1.000000000000000000, 0.9807852804032304306, 1.000000000000000000, 0.9807852804032304306, 1.000000000000000000, 0.9807852804032304306, 1.000000000000000000, 0.9807852804032270999, 1.000000000000003331 ) ) 
 REPRESENTATION_ITEM ( '' )  );
#12933 = CARTESIAN_POINT ( 'NONE',  ( -19.19641293061498999, 408.8073905683720000, 14.20200298773971426 ) ) ;
#12934 = CARTESIAN_POINT ( 'NONE',  ( -11.93348319268870661, 250.3698905683720000, -2.051577885510841163E-15 ) ) ;
#12935 = EDGE_CURVE ( 'NONE', #10361, #9753, #17489, .T. ) ;
#12936 = ORIENTED_EDGE ( 'NONE', *, *, #19928, .T. ) ;
#12937 = ORIENTED_EDGE ( 'NONE', *, *, #15923, .T. ) ;
#12938 = CARTESIAN_POINT ( 'NONE',  ( 5.074999999999999289, 6.500000000000000888, 0.000000000000000000 ) ) ;
#12939 = ORIENTED_EDGE ( 'NONE', *, *, #12800, .F. ) ;
#12940 = CARTESIAN_POINT ( 'NONE',  ( -45.43829269268872650, 455.3698905683720000, 0.000000000000000000 ) ) ;
#12941 = CARTESIAN_POINT ( 'NONE',  ( -47.16347859291443001, 221.3698905765656377, -7.653668647301793193 ) ) ;
#12942 = ORIENTED_EDGE ( 'NONE', *, *, #10887, .F. ) ;
#12943 = CARTESIAN_POINT ( 'NONE',  ( -42.99872675744465766, 207.3681867157733052, 4.490020761129740912 ) ) ;
#12944 = CARTESIAN_POINT ( 'NONE',  ( -38.17536295476243424, 225.4323905683720000, 14.20200298773971781 ) ) ;
#12945 = ORIENTED_EDGE ( 'NONE', *, *, #6703, .T. ) ;
#12946 = CARTESIAN_POINT ( 'NONE',  ( -44.16309181155859420, 513.2448905683719431, -6.410867750099231266 ) ) ;
#12947 = CARTESIAN_POINT ( 'NONE',  ( 0.000000000000000000, 10.52886280891152104, 0.000000000000000000 ) ) ;
#12948 = CARTESIAN_POINT ( 'NONE',  ( -24.70764059509556176, 444.8073905765655809, 19.99999999999998934 ) ) ;
#12949 = CARTESIAN_POINT ( 'NONE',  ( -48.68588794268853803, 301.6823905765655809, -3.978247347593583783 ) ) ;
#12950 = CARTESIAN_POINT ( 'NONE',  ( -13.20868407381885667, 348.2448905683720000, 6.410867750099229490 ) ) ;
#12951 = CARTESIAN_POINT ( 'NONE',  ( -17.35679799567828141, 238.5573905765656093, -16.95518130045146421 ) ) ;
#12952 = CARTESIAN_POINT ( 'NONE',  ( -42.82802356641965247, 288.4948905601785327, 14.14213562373094923 ) ) ;
#12953 = SURFACE_SIDE_STYLE ('',( #9159 ) ) ;
#12954 = CARTESIAN_POINT ( 'NONE',  ( -45.43829269268869098, 224.1823905683720284, 3.332260488124734632 ) ) ;
#12955 = CARTESIAN_POINT ( 'NONE',  ( -38.17536295476244135, 316.9323905683719431, 14.20200298773971781 ) ) ;
#12956 = LINE ( 'NONE', #3114, #10916 ) ;
#12957 = FACE_OUTER_BOUND ( 'NONE', #6081, .T. ) ;
#12958 = CARTESIAN_POINT ( 'NONE',  ( -19.19641293061497578, 298.8073905683719431, 14.20200298773971426 ) ) ;
#12959 = CARTESIAN_POINT ( 'NONE',  ( -35.09675569278797269, 517.2448905683719431, 15.47720386886985366 ) ) ;
#12960 = CARTESIAN_POINT ( 'NONE',  ( -40.01497788969913927, 365.6823905601784759, -16.95518130045146421 ) ) ;
#12961 = CARTESIAN_POINT ( 'NONE',  ( -47.16347859291443001, 231.3698905765656093, -7.653668647301793193 ) ) ;
#12962 = VERTEX_POINT ( 'NONE', #20585 ) ;
#12963 = CARTESIAN_POINT ( 'NONE',  ( -25.35362745456400901, 492.5573905683721136, -16.75240474999999307 ) ) ;
#12964 = CARTESIAN_POINT ( 'NONE',  ( 115.7989814974898337, 152.5259582928263740, 40.00000000000000000 ) ) ;
#12965 = CARTESIAN_POINT ( 'NONE',  ( -42.88789093042842637, 282.9323905683721136, -9.489475012073736337 ) ) ;
#12966 = VERTEX_POINT ( 'NONE', #387 ) ;
#12967 = CARTESIAN_POINT ( 'NONE',  ( -42.88789093042842637, 286.3073905683720000, 9.489475012073734561 ) ) ;
#12968 = CARTESIAN_POINT ( 'NONE',  ( -16.84014894278198327, 317.6198905683720568, 11.84573899990672530 ) ) ;
#12969 = CARTESIAN_POINT ( 'NONE',  ( -42.88789093042841927, 266.3073905683720568, 9.489475012073734561 ) ) ;
#12970 = CARTESIAN_POINT ( 'NONE',  ( -32.66413529028186247, 264.1823905765656377, 19.99999999999999289 ) ) ;
#12971 = CARTESIAN_POINT ( 'NONE',  ( -11.73070664223726389, 473.1823905601784759, -11.32908994701042538 ) ) ;
#12972 = CARTESIAN_POINT ( 'NONE',  ( -22.27502019258947286, 230.7448905683720000, -15.47720386886985544 ) ) ;
#12973 = CARTESIAN_POINT ( 'NONE',  ( -32.01814843081344719, 387.5573905683719431, 16.75240474999999307 ) ) ;
#12974 = DIRECTION ( 'NONE',  ( -1.191790137725560488E-16, 1.000000000000000000, 0.000000000000000000 ) ) ;
#12975 = CARTESIAN_POINT ( 'NONE',  ( -8.685887942688886199, 261.9323905601784759, 3.978247347593586447 ) ) ;
#12976 = ADVANCED_FACE ( 'NONE', ( #13894 ), #20371, .T. ) ;
#12977 = CARTESIAN_POINT ( 'NONE',  ( -11.73070664223723902, 267.9323905765656377, -11.32908994701042538 ) ) ;
#12978 = CARTESIAN_POINT ( 'NONE',  ( -35.09675569278795138, 431.9948905683720568, -15.47720386886985544 ) ) ;
#12979 = FACE_OUTER_BOUND ( 'NONE', #2811, .T. ) ;
#12980 = ORIENTED_EDGE ( 'NONE', *, *, #8218, .T. ) ;
#12981 = CARTESIAN_POINT ( 'NONE',  ( -48.68588794268871567, 416.9323905601784759, -3.978247347593158345 ) ) ;
#12982 = ORIENTED_EDGE ( 'NONE', *, *, #13913, .T. ) ;
#12983 = ORIENTED_EDGE ( 'NONE', *, *, #13198, .F. ) ;
#12984 = VERTEX_POINT ( 'NONE', #3819 ) ;
#12985 = CARTESIAN_POINT ( 'NONE',  ( 51.98438129372387806, -133.1434774248255906, -94.99999999999994316 ) ) ;
#12986 = CARTESIAN_POINT ( 'NONE',  ( -14.54375231895775933, 300.9948905601784759, 14.14213562373094568 ) ) ;
#12987 = CARTESIAN_POINT ( 'NONE',  ( 118.4271928232701043, 31.85652257517428865, 40.00000000000000711 ) ) ;
#12988 = CARTESIAN_POINT ( 'NONE',  ( -28.68588794268871567, 352.8698905683720568, -16.75240474999999307 ) ) ;
#12989 = CARTESIAN_POINT ( 'NONE',  ( -11.73070664223726745, 507.9323905765655809, -11.32908994701042715 ) ) ;
#12990 = CARTESIAN_POINT ( 'NONE',  ( -14.48388495494900141, 387.9323905683720000, 9.489475012073732785 ) ) ;
#12991 = CARTESIAN_POINT ( 'NONE',  ( -35.09675569278793006, 223.4948905683720284, -15.47720386886985544 ) ) ;
#12992 = CARTESIAN_POINT ( 'NONE',  ( -13.20868407381886378, 389.4948905683720000, -6.410867750099233042 ) ) ;
#12993 = ADVANCED_FACE ( 'NONE', ( #8686 ), #5334, .F. ) ;
#12994 = VECTOR ( 'NONE', #11047, 1000.000000000000000 ) ;
#12995 = CARTESIAN_POINT ( 'NONE',  ( -36.33955658999050797, 323.8698905765656377, 18.47759065022572500 ) ) ;
#12996 = CARTESIAN_POINT ( 'NONE',  ( 45.67500000000000426, 0.000000000000000000, 0.000000000000000000 ) ) ;
#12997 = CARTESIAN_POINT ( 'NONE',  ( -19.19641293061496867, 277.3073905683720000, 14.20200298773971426 ) ) ;
#12998 =( LENGTH_UNIT ( ) NAMED_UNIT ( * ) SI_UNIT ( .MILLI., .METRE. ) );
#12999 = CARTESIAN_POINT ( 'NONE',  ( -40.53162694259544452, 446.6198905683720568, 11.84573899990672885 ) ) ;
#13000 = AXIS2_PLACEMENT_3D ( 'NONE', #13115, #15973, #13337 ) ;
#13001 = CYLINDRICAL_SURFACE ( 'NONE', #16158, 50.00000000000000000 ) ;
#13002 = CARTESIAN_POINT ( 'NONE',  ( -21.03221929538692692, 500.3698905601785327, 18.47759065022572500 ) ) ;
#13003 = LINE ( 'NONE', #8445, #12313 ) ;
#13004 = CARTESIAN_POINT ( 'NONE',  ( -16.84014894278198682, 349.1198905683720568, 11.84573899990672530 ) ) ;
#13005 = CARTESIAN_POINT ( 'NONE',  ( -45.43829269268871940, 474.1823905683720000, 3.332260488124734632 ) ) ;
#13006 = CARTESIAN_POINT ( 'NONE',  ( -47.16347859291445843, 486.6198905601784759, -7.653668647301793193 ) ) ;
#13007 = CARTESIAN_POINT ( 'NONE',  ( -11.93348319268871904, 329.1823905683720568, -3.332260488124732856 ) ) ;
#13008 = EDGE_CURVE ( 'NONE', #19239, #16434, #8745, .T. ) ;
#13009 = AXIS2_PLACEMENT_3D ( 'NONE', #21253, #21042, #3086 ) ;
#13010 = ORIENTED_EDGE ( 'NONE', *, *, #1603, .T. ) ;
#13011 = DIRECTION ( 'NONE',  ( 0.000000000000000000, -1.000000000000000000, 0.000000000000000000 ) ) ;
#13012 = ORIENTED_EDGE ( 'NONE', *, *, #16425, .T. ) ;
#13013 = CARTESIAN_POINT ( 'NONE',  ( -29.48036301152122718, 47.76573509908928372, 49.60091809715360966 ) ) ;
#13014 = CIRCLE ( 'NONE', #17506, 6.500000000000000888 ) ;
#13015 = CARTESIAN_POINT ( 'NONE',  ( -14.48388495494900674, 409.4323905683720568, 9.489475012073731008 ) ) ;
#13016 = PLANE ( 'NONE',  #12117 ) ;
#13017 = CARTESIAN_POINT ( 'NONE',  ( 65.85920792673738333, 160.1716627696692683, 40.00000000000000000 ) ) ;
#13018 = CARTESIAN_POINT ( 'NONE',  ( -45.43829269268871229, 444.1823905683719431, 3.332260488124734632 ) ) ;
#13019 = CARTESIAN_POINT ( 'NONE',  ( -45.43829269268872650, 454.1823905683720568, 3.332260488124734632 ) ) ;
#13020 = DIRECTION ( 'NONE',  ( -1.191790137725560488E-16, 1.000000000000000000, -0.000000000000000000 ) ) ;
#13021 = EDGE_CURVE ( 'NONE', #17195, #19655, #16821, .T. ) ;
#13022 = CARTESIAN_POINT ( 'NONE',  ( -8.685887942688722774, 376.6823905765656946, 3.978247347593161010 ) ) ;
#13023 = CARTESIAN_POINT ( 'NONE',  ( -12.95795174569926722, 50.01372181642471304, 47.04466289070994378 ) ) ;
#13024 = CARTESIAN_POINT ( 'NONE',  ( -32.66413529028187668, 389.8073905765656377, -19.99999999999999289 ) ) ;
#13025 = CARTESIAN_POINT ( 'NONE',  ( -17.35679799567830273, 428.5573905765656377, -16.95518130045146421 ) ) ;
#13026 = CARTESIAN_POINT ( 'NONE',  ( -28.68588794268874054, 573.2448905601785327, 0.000000000000000000 ) ) ;
#13027 = CARTESIAN_POINT ( 'NONE',  ( -11.93348319268873681, 490.6823905683720568, -3.332260488124732856 ) ) ;
#13028 = AXIS2_PLACEMENT_3D ( 'NONE', #9113, #15734, #18532 ) ;
#13029 = CARTESIAN_POINT ( 'NONE',  ( 20.60949999999999349, 0.000000000000000000, 0.000000000000000000 ) ) ;
#13030 = CARTESIAN_POINT ( 'NONE',  ( -123.2946569474810303, 10.52886280891152104, -20.57735571454641388 ) ) ;
#13031 = DIRECTION ( 'NONE',  ( 0.000000000000000000, 0.000000000000000000, 1.000000000000000000 ) ) ;
#13032 =( REPRESENTATION_RELATIONSHIP ('NONE','NONE', #1888, #4076 ) REPRESENTATION_RELATIONSHIP_WITH_TRANSFORMATION ( #15508 )SHAPE_REPRESENTATION_RELATIONSHIP( ) );
#13033 = AXIS2_PLACEMENT_3D ( 'NONE', #19156, #7673, #12659 ) ;
#13034 = CARTESIAN_POINT ( 'NONE',  ( -40.53162694259544452, 404.1198905683720000, -11.84573899990672707 ) ) ;
#13035 = CARTESIAN_POINT ( 'NONE',  ( -8.685887942688729879, 436.9948905765656377, -2.449293598294705724E-15 ) ) ;
#13036 = CARTESIAN_POINT ( 'NONE',  ( -35.09675569278793716, 237.2448905683720000, 15.47720386886985366 ) ) ;
#13037 = ORIENTED_EDGE ( 'NONE', *, *, #14268, .F. ) ;
#13038 = CARTESIAN_POINT ( 'NONE',  ( -17.35679799567829562, 425.4323905765656377, 16.95518130045146421 ) ) ;
#13039 = ORIENTED_EDGE ( 'NONE', *, *, #16657, .T. ) ;
#13040 = CARTESIAN_POINT ( 'NONE',  ( -25.35362745456400191, 462.5573905683720568, -16.75240474999999307 ) ) ;
#13041 = CARTESIAN_POINT ( 'NONE',  ( -48.68588794268869435, 232.3073905765656377, 3.978247347593168115 ) ) ;
#13042 = AXIS2_PLACEMENT_3D ( 'NONE', #1926, #5254, #8493 ) ;
#13043 = ORIENTED_EDGE ( 'NONE', *, *, #15071, .T. ) ;
#13044 = CYLINDRICAL_SURFACE ( 'NONE', #12111, 43.46661168214937732 ) ;
#13045 = CARTESIAN_POINT ( 'NONE',  ( -25.35362745456397349, 221.0573905683720284, -16.75240474999999307 ) ) ;
#13046 = ORIENTED_EDGE ( 'NONE', *, *, #16507, .T. ) ;
#13047 = CARTESIAN_POINT ( 'NONE',  ( -11.93348319268873858, 508.8698905683719431, -2.051577885510841163E-15 ) ) ;
#13048 = DIRECTION ( 'NONE',  ( -0.000000000000000000, 0.8660254037844383745, 0.5000000000000004441 ) ) ;
#13049 = CARTESIAN_POINT ( 'NONE',  ( -10.20829729246299600, 437.6198905765656377, -7.653668647301794969 ) ) ;
#13050 = PRODUCT_DEFINITION_SHAPE ( 'NONE', 'NONE',  #21395 ) ;
#13051 = CARTESIAN_POINT ( 'NONE',  ( 0.05458999538792623507, -1.264741368075137817, 6.499999999999999112 ) ) ;
#13052 = CARTESIAN_POINT ( 'NONE',  ( -8.685887942688708563, 246.9948905765656093, -2.449293598294705724E-15 ) ) ;
#13053 = CARTESIAN_POINT ( 'NONE',  ( -10.20829729246299777, 456.3698905765656377, 7.653668647301790529 ) ) ;
#13054 = DIRECTION ( 'NONE',  ( 1.191790137725560488E-16, -1.000000000000000000, -0.000000000000000000 ) ) ;
#13055 = EDGE_CURVE ( 'NONE', #5825, #3667, #8843, .T. ) ;
#13056 = DIRECTION ( 'NONE',  ( 0.000000000000000000, 0.000000000000000000, -1.000000000000000000 ) ) ;
#13057 =( BOUNDED_CURVE ( )  B_SPLINE_CURVE ( 2, ( #13459, #3076, #11285, #17883, #16494, #8033, #5121, #13024, #9659, #14664, #1791, #21245, #169, #6410, #6739, #11721, #5228 ),
 .UNSPECIFIED., .F., .T. ) 
 B_SPLINE_CURVE_WITH_KNOTS ( ( 3, 2, 2, 2, 2, 2, 2, 2, 3 ),
 ( 0.4375000000000002220, 0.4394531250000002220, 0.4414062500000002220, 0.4433593750000002220, 0.4453125000000002220, 0.4472656250000002220, 0.4492187500000002220, 0.4511718750000002220, 0.4531250000000002220 ),
 .UNSPECIFIED. ) 
 CURVE ( )  GEOMETRIC_REPRESENTATION_ITEM ( )  RATIONAL_B_SPLINE_CURVE ( ( 0.9999999999999977796, 0.9807852804032326510, 1.000000000000000000, 0.9807852804032304306, 1.000000000000000000, 0.9807852804032304306, 1.000000000000000000, 0.9807852804032304306, 1.000000000000000000, 0.9807852804032304306, 1.000000000000000000, 0.9807852804032304306, 1.000000000000000000, 0.9807852804032304306, 1.000000000000000000, 0.9807852804032282101, 1.000000000000002220 ) ) 
 REPRESENTATION_ITEM ( '' )  );
#13058 = EDGE_CURVE ( 'NONE', #8642, #6189, #9566, .T. ) ;
#13059 = CARTESIAN_POINT ( 'NONE',  ( 40.42502041961814996, 170.1716627696692683, 40.00000000000000000 ) ) ;
#13060 = CARTESIAN_POINT ( 'NONE',  ( -8.915191811234558728, 223.9102039777117739, -3.487082981424983519 ) ) ;
#13061 = CARTESIAN_POINT ( 'NONE',  ( -35.09675569278793716, 313.4948905683720000, -15.47720386886985544 ) ) ;
#13062 = FACE_OUTER_BOUND ( 'NONE', #1311, .T. ) ;
#13063 = CARTESIAN_POINT ( 'NONE',  ( -10.20829729246297468, 261.6198905601784759, 7.653668647301790529 ) ) ;
#13064 = CARTESIAN_POINT ( 'NONE',  ( -14.54375231895776821, 380.9948905601784759, 14.14213562373094568 ) ) ;
#13065 = CARTESIAN_POINT ( 'NONE',  ( -32.01814843081344009, 293.1823905683720568, -16.75240474999999307 ) ) ;
#13066 = EDGE_CURVE ( 'NONE', #15561, #19827, #17029, .T. ) ;
#13067 = CARTESIAN_POINT ( 'NONE',  ( -42.88789093042845479, 516.3073905683720568, 9.489475012073734561 ) ) ;
#13068 = CARTESIAN_POINT ( 'NONE',  ( -32.66413529028187668, 359.4323905601784759, 19.99999999999999289 ) ) ;
#13069 = EDGE_CURVE ( 'NONE', #15822, #11300, #2317, .T. ) ;
#13070 = CARTESIAN_POINT ( 'NONE',  ( -11.73070664223724613, 313.1823905601784190, -11.32908994701042538 ) ) ;
#13071 = ORIENTED_EDGE ( 'NONE', *, *, #8287, .T. ) ;
#13072 = CARTESIAN_POINT ( 'NONE',  ( -38.17536295476246266, 496.9323905683720568, 14.20200298773971781 ) ) ;
#13073 = DIRECTION ( 'NONE',  ( -0.000000000000000000, -0.000000000000000000, 1.000000000000000000 ) ) ;
#13074 = CARTESIAN_POINT ( 'NONE',  ( -28.68588794268870501, 281.3698905683720000, -16.75240474999999307 ) ) ;
#13075 = EDGE_LOOP ( 'NONE', ( #15978, #10628, #11866, #1631 ) ) ;
#13076 = CARTESIAN_POINT ( 'NONE',  ( -40.53162694259543031, 276.6198905683720568, 11.84573899990672885 ) ) ;
#13077 = CARTESIAN_POINT ( 'NONE',  ( -45.43829269268869808, 313.5573905683720000, -3.332260488124726194 ) ) ;
#13078 = CARTESIAN_POINT ( 'NONE',  ( -13.20868407381884779, 259.7448905683720000, 6.410867750099229490 ) ) ;
#13079 = EDGE_CURVE ( 'NONE', #15843, #5613, #924, .T. ) ;
#13080 = CARTESIAN_POINT ( 'NONE',  ( -14.54375231895775222, 245.7448905765656093, 14.14213562373094568 ) ) ;
#13081 = CARTESIAN_POINT ( 'NONE',  ( -28.68588794268873698, 548.2448905601784190, 0.000000000000000000 ) ) ;
#13082 = CARTESIAN_POINT ( 'NONE',  ( -22.30770786884145451, 30.52886280891152282, 122.9933582338429972 ) ) ;
#13083 = CARTESIAN_POINT ( 'NONE',  ( -19.19641293061498644, 378.8073905683721136, 14.20200298773971426 ) ) ;
#13084 = CARTESIAN_POINT ( 'NONE',  ( -10.20829729246297646, 281.6198905601784759, 7.653668647301790529 ) ) ;
#13085 = CARTESIAN_POINT ( 'NONE',  ( -42.82802356641967378, 460.7448905765655809, -14.14213562373094746 ) ) ;
#13086 = CARTESIAN_POINT ( 'NONE',  ( -14.54375231895775933, 268.2448905765656377, -14.14213562373094746 ) ) ;
#13087 = CIRCLE ( 'NONE', #19290, 6.500000000000000888 ) ;
#13088 = CARTESIAN_POINT ( 'NONE',  ( -16.84014894278199748, 420.1198905683720000, -11.84573899990672707 ) ) ;
#13089 = UNCERTAINTY_MEASURE_WITH_UNIT (LENGTH_MEASURE( 1.000000000000000082E-05 ), #13667, 'distance_accuracy_value', 'NONE');
#13090 = DIRECTION ( 'NONE',  ( -0.8090169943749473402, 0.000000000000000000, 0.5877852522924732481 ) ) ;
#13091 = ORIENTED_EDGE ( 'NONE', *, *, #2847, .F. ) ;
#13092 = CARTESIAN_POINT ( 'NONE',  ( -17.35679799567830628, 423.8073905601784759, -16.95518130045146421 ) ) ;
#13093 = ORIENTED_EDGE ( 'NONE', *, *, #15327, .F. ) ;
#13094 = CARTESIAN_POINT ( 'NONE',  ( 0.5805565836007597902, 3.752776749732560368, -6.499999999999999112 ) ) ;
#13095 = ORIENTED_EDGE ( 'NONE', *, *, #14597, .T. ) ;
#13096 = EDGE_LOOP ( 'NONE', ( #850, #6533, #14086, #17409 ) ) ;
#13097 = FACE_BOUND ( 'NONE', #16771, .T. ) ;
#13098 = CARTESIAN_POINT ( 'NONE',  ( -48.68588794268870146, 297.5573905601785327, 3.978247347593168115 ) ) ;
#13099 = PLANE ( 'NONE',  #4538 ) ;
#13100 = CARTESIAN_POINT ( 'NONE',  ( -44.16309181155856578, 345.9948905683720000, 6.410867750099241924 ) ) ;
#13101 = EDGE_CURVE ( 'NONE', #13316, #15497, #19385, .T. ) ;
#13102 = CARTESIAN_POINT ( 'NONE',  ( -42.82802356641967378, 490.7448905765656377, -14.14213562373094746 ) ) ;
#13103 = CARTESIAN_POINT ( 'NONE',  ( -45.43829269268870519, 364.1823905683720568, 3.332260488124734632 ) ) ;
#13104 = DIRECTION ( 'NONE',  ( 0.000000000000000000, -1.000000000000000000, 0.000000000000000000 ) ) ;
#13105 = CARTESIAN_POINT ( 'NONE',  ( -35.09675569278794427, 381.9948905683720568, -15.47720386886985544 ) ) ;
#13106 = AXIS2_PLACEMENT_3D ( 'NONE', #2737, #4025, #9211 ) ;
#13107 = CARTESIAN_POINT ( 'NONE',  ( -28.68588794268870856, 314.4948905765656377, 19.99999999999999289 ) ) ;
#13108 = CARTESIAN_POINT ( 'NONE',  ( 5.074999999999999289, 3.752776749732562589, 6.500000000000000000 ) ) ;
#13109 = CARTESIAN_POINT ( 'NONE',  ( -45.43829269268870519, 294.1823905683720568, 3.332260488124734632 ) ) ;
#13110 = DIRECTION ( 'NONE',  ( 0.000000000000000000, 0.000000000000000000, -1.000000000000000000 ) ) ;
#13111 = CARTESIAN_POINT ( 'NONE',  ( -13.20868407381886911, 430.9948905683720568, -6.410867750099233042 ) ) ;
#13112 = DIRECTION ( 'NONE',  ( -0.000000000000000000, 1.000000000000000000, -0.000000000000000000 ) ) ;
#13113 = CARTESIAN_POINT ( 'NONE',  ( 20.42502041961813930, 230.5765313837437418, 40.00000000000000000 ) ) ;
#13114 = CARTESIAN_POINT ( 'NONE',  ( -48.68588794268869435, 227.2448905601785043, 0.000000000000000000 ) ) ;
#13115 = CARTESIAN_POINT ( 'NONE',  ( 0.000000000000000000, 0.000000000000000000, 0.000000000000000000 ) ) ;
#13116 = CARTESIAN_POINT ( 'NONE',  ( -35.09675569278795138, 357.2448905683720000, 15.47720386886985366 ) ) ;
#13117 = CARTESIAN_POINT ( 'NONE',  ( -25.35362745456400901, 491.0573905683720000, -16.75240474999999307 ) ) ;
#13118 = ORIENTED_EDGE ( 'NONE', *, *, #20988, .F. ) ;
#13119 = CARTESIAN_POINT ( 'NONE',  ( -36.33955658999052218, 485.3698905601784759, -18.47759065022572855 ) ) ;
#13120 = CARTESIAN_POINT ( 'NONE',  ( -40.53162694259543031, 305.1198905683720000, 11.84573899990672885 ) ) ;
#13121 = AXIS2_PLACEMENT_3D ( 'NONE', #3027, #56, #20981 ) ;
#13122 = EDGE_CURVE ( 'NONE', #4584, #7636, #4356, .T. ) ;
#13123 = ORIENTED_EDGE ( 'NONE', *, *, #11412, .F. ) ;
#13124 = CARTESIAN_POINT ( 'NONE',  ( -36.33955658999052929, 525.3698905601784190, -18.47759065022572855 ) ) ;
#13125 = ORIENTED_EDGE ( 'NONE', *, *, #8950, .F. ) ;
#13126 = CARTESIAN_POINT ( 'NONE',  ( -31.45575705393271448, 49.80536212050644451, 49.52427915835843208 ) ) ;
#13127 = CARTESIAN_POINT ( 'NONE',  ( -25.35362745456398414, 398.1823905683720568, 16.75240474999998952 ) ) ;
#13128 = CARTESIAN_POINT ( 'NONE',  ( 0.5805565836007702263, -7.505553499465148271, -1.692530754021427292E-16 ) ) ;
#13129 =( NAMED_UNIT ( * ) PLANE_ANGLE_UNIT ( ) SI_UNIT ( $, .RADIAN. ) );
#13130 = CARTESIAN_POINT ( 'NONE',  ( -19.19641293061499354, 450.4323905683720000, -14.20200298773971603 ) ) ;
#13131 = CARTESIAN_POINT ( 'NONE',  ( -13.20868407381887089, 439.4948905683720568, -6.410867750099233042 ) ) ;
#13132 = DIRECTION ( 'NONE',  ( 0.000000000000000000, 0.000000000000000000, -1.000000000000000000 ) ) ;
#13133 = CARTESIAN_POINT ( 'NONE',  ( -40.01497788969913927, 380.4323905765655240, -16.95518130045146421 ) ) ;
#13134 = CARTESIAN_POINT ( 'NONE',  ( 43.53705524234220547, 56.85652257517428865, 96.62835994548002816 ) ) ;
#13135 = FACE_OUTER_BOUND ( 'NONE', #11226, .T. ) ;
#13136 = CYLINDRICAL_SURFACE ( 'NONE', #10133, 20.00000000000000000 ) ;
#13137 = CARTESIAN_POINT ( 'NONE',  ( -8.685887942688736985, 486.9948905765656377, -2.449293598294705724E-15 ) ) ;
#13138 = CARTESIAN_POINT ( 'NONE',  ( -13.20868407381887621, 490.9948905683720568, -6.410867750099233042 ) ) ;
#13139 = EDGE_CURVE ( 'NONE', #4779, #5825, #5052, .T. ) ;
#13140 = DIRECTION ( 'NONE',  ( 0.4627175328665443232, 5.514621922230504147E-17, -0.8865057725575725689 ) ) ;
#13141 = CARTESIAN_POINT ( 'NONE',  ( 35.96497763894178945, 230.5765313837437418, 40.00000000000000000 ) ) ;
#13142 = CARTESIAN_POINT ( 'NONE',  ( -22.30770786884145451, 10.52886280891152104, 122.9933582338429972 ) ) ;
#13143 = CARTESIAN_POINT ( 'NONE',  ( -19.19641293061498999, 401.9323905683720000, -14.20200298773971603 ) ) ;
#13144 = CARTESIAN_POINT ( 'NONE',  ( -10.20829729246299955, 467.6198905765656377, -7.653668647301794969 ) ) ;
#13145 = CLOSED_SHELL ( 'NONE', ( #5860, #9074, #13382, #338, #5918, #19214, #17161, #6001, #11530, #15312, #3749, #7038, #21298, #3277, #14413, #5470, #8687, #1178, #3546, #4917, #20072, #10754, #5614, #855, #5602, #17811, #19921, #15767, #3788 ) ) ;
#13146 = CARTESIAN_POINT ( 'NONE',  ( -13.20868407381884424, 229.7448905683720568, 6.410867750099229490 ) ) ;
#13147 = EDGE_CURVE ( 'NONE', #13610, #2785, #4570, .T. ) ;
#13148 = ORIENTED_EDGE ( 'NONE', *, *, #12393, .F. ) ;
#13149 = CYLINDRICAL_SURFACE ( 'NONE', #3066, 15.00000000000000355 ) ;
#13150 = VERTEX_POINT ( 'NONE', #12476 ) ;
#13151 = CARTESIAN_POINT ( 'NONE',  ( -44.16309181155857999, 434.7448905683720000, -6.410867750099231266 ) ) ;
#13152 = CARTESIAN_POINT ( 'NONE',  ( -21.03221929538689849, 235.1198905765656377, 18.47759065022572500 ) ) ;
#13153 = CONICAL_SURFACE ( 'NONE', #19700, 6.500000000000000000, 1.047197551196600296 ) ;
#13154 = ORIENTED_EDGE ( 'NONE', *, *, #15729, .F. ) ;
#13155 = DIRECTION ( 'NONE',  ( 0.000000000000000000, 0.000000000000000000, -1.000000000000000000 ) ) ;
#13156 = CARTESIAN_POINT ( 'NONE',  ( -38.17536295476247687, 533.8073905683720568, -14.20200298773971426 ) ) ;
#13157 = VERTEX_POINT ( 'NONE', #14433 ) ;
#13158 = CARTESIAN_POINT ( 'NONE',  ( -45.43829269268873361, 513.5573905683720568, -3.332260488124726638 ) ) ;
#13159 = CARTESIAN_POINT ( 'NONE',  ( 2.416697501590669095, 172.9933428177121471, -45.00000000000000000 ) ) ;
#13160 = VECTOR ( 'NONE', #3205, 1000.000000000000000 ) ;
#13162 = AXIS2_PLACEMENT_3D ( 'NONE', #6398, #13011, #4780 ) ;
#13161 = CARTESIAN_POINT ( 'NONE',  ( -32.66413529028189089, 449.8073905765656946, -19.99999999999999289 ) ) ;
#13163 = CARTESIAN_POINT ( 'NONE',  ( 146.3141120573112630, 610.7448905601785327, 0.000000000000000000 ) ) ;
#13164 = CARTESIAN_POINT ( 'NONE',  ( -10.20829729246298179, 331.6198905601784759, 7.653668647301790529 ) ) ;
#13165 = CARTESIAN_POINT ( 'NONE',  ( -28.68588794268872633, 378.8848358243226357, -38.00000000000000000 ) ) ;
#13166 = CIRCLE ( 'NONE', #15240, 53.46661168214943416 ) ;
#13167 = CARTESIAN_POINT ( 'NONE',  ( -21.03221929538690915, 238.8698905765656093, -18.47759065022572855 ) ) ;
#13168 = DIRECTION ( 'NONE',  ( -0.000000000000000000, -1.000000000000000000, -0.000000000000000000 ) ) ;
#13169 = CARTESIAN_POINT ( 'NONE',  ( 51.50493485826542184, 141.8799693780962912, -94.99999999999994316 ) ) ;
#13170 = CARTESIAN_POINT ( 'NONE',  ( -18.66797547166049753, 223.9102039777116602, -17.31025331282116397 ) ) ;
#13171 = CARTESIAN_POINT ( 'NONE',  ( -44.16309181155856578, 324.7448905683720000, -6.410867750099231266 ) ) ;
#13172 = CARTESIAN_POINT ( 'NONE',  ( -47.16347859291443001, 236.6198905601784475, -7.653668647301793193 ) ) ;
#13173 = PRODUCT_DEFINITION_FORMATION_WITH_SPECIFIED_SOURCE ( 'ANY', '', #15993, .NOT_KNOWN. ) ;
#13174 = CARTESIAN_POINT ( 'NONE',  ( -10.20829729246297468, 262.8698905601785327, -7.653668647301794969 ) ) ;
#13175 = CARTESIAN_POINT ( 'NONE',  ( 0.000000000000000000, 135.1716627696692683, -33.59072564020503648 ) ) ;
#13176 = CARTESIAN_POINT ( 'NONE',  ( -28.68588794268870501, 282.8698905683720568, -16.75240474999999307 ) ) ;
#13177=STYLED_ITEM('',(#21421),#12161);
#13178 = CARTESIAN_POINT ( 'NONE',  ( -28.68588794268873343, 512.8698905683719431, -16.75240474999999307 ) ) ;
#13179 = CARTESIAN_POINT ( 'NONE',  ( -40.01497788969913216, 368.8073905601785327, 16.95518130045146776 ) ) ;
#13180 = DIRECTION ( 'NONE',  ( -1.000000000000000000, 0.000000000000000000, -8.901024030850960568E-17 ) ) ;
#13181 = ORIENTED_EDGE ( 'NONE', *, *, #16163, .T. ) ;
#13182 = CARTESIAN_POINT ( 'NONE',  ( -13.20868407381887444, 489.7448905683720568, 6.410867750099229490 ) ) ;
#13183 = DIRECTION ( 'NONE',  ( 0.6352526299242177155, 0.000000000000000000, 0.7723044064191041391 ) ) ;
#13184 = CARTESIAN_POINT ( 'NONE',  ( -38.17536295476244135, 275.4323905683720568, 14.20200298773971781 ) ) ;
#13185 = VERTEX_POINT ( 'NONE', #6183 ) ;
#13186 =( BOUNDED_CURVE ( )  B_SPLINE_CURVE ( 2, ( #20309, #8406, #8829, #13401, #7199, #19988, #15030, #15351, #11973, #16652, #5168, #13507, #1943, #16756, #18359, #3859, #8511 ),
 .UNSPECIFIED., .F., .T. ) 
 B_SPLINE_CURVE_WITH_KNOTS ( ( 3, 2, 2, 2, 2, 2, 2, 2, 3 ),
 ( 0.3750000000000001665, 0.3769531250000001665, 0.3789062500000001665, 0.3808593750000001665, 0.3828125000000001665, 0.3847656250000001665, 0.3867187500000001665, 0.3886718750000001665, 0.3906250000000001665 ),
 .UNSPECIFIED. ) 
 CURVE ( )  GEOMETRIC_REPRESENTATION_ITEM ( )  RATIONAL_B_SPLINE_CURVE ( ( 0.9999999999999983347, 0.9807852804032320959, 1.000000000000000000, 0.9807852804032304306, 1.000000000000000000, 0.9807852804032304306, 1.000000000000000000, 0.9807852804032304306, 1.000000000000000000, 0.9807852804032304306, 1.000000000000000000, 0.9807852804032304306, 1.000000000000000000, 0.9807852804032304306, 1.000000000000000000, 0.9807852804032287652, 1.000000000000001554 ) ) 
 REPRESENTATION_ITEM ( '' )  );
#13187 = CARTESIAN_POINT ( 'NONE',  ( 60.03793209889851568, 30.52886280891152282, 131.1729372809869005 ) ) ;
#13188 = CARTESIAN_POINT ( 'NONE',  ( -40.53162694259543031, 274.1198905683720568, -11.84573899990672707 ) ) ;
#13189 = CARTESIAN_POINT ( 'NONE',  ( -44.16309181155855867, 254.7448905683720284, -6.410867750099231266 ) ) ;
#13190 = ADVANCED_FACE ( 'NONE', ( #17342 ), #21014, .T. ) ;
#13191 = CARTESIAN_POINT ( 'NONE',  ( -11.73070664223723547, 247.9323905765656377, -11.32908994701042715 ) ) ;
#13192 = CARTESIAN_POINT ( 'NONE',  ( -36.33955658999052218, 475.3698905601784759, -18.47759065022572855 ) ) ;
#13193 = AXIS2_PLACEMENT_3D ( 'NONE', #5715, #10684, #15584 ) ;
#13194 = DIRECTION ( 'NONE',  ( 0.000000000000000000, 1.000000000000000000, 0.000000000000000000 ) ) ;
#13195 = CARTESIAN_POINT ( 'NONE',  ( -19.19641293061497223, 267.3073905683720568, 14.20200298773971426 ) ) ;
#13196 = EDGE_CURVE ( 'NONE', #13742, #15419, #8508, .T. ) ;
#13197 = CARTESIAN_POINT ( 'NONE',  ( -40.53162694259543741, 384.1198905683720568, -11.84573899990672707 ) ) ;
#13198 = EDGE_CURVE ( 'NONE', #18325, #7334, #11160, .T. ) ;
#13199 = CARTESIAN_POINT ( 'NONE',  ( -43.04611869048239470, 202.6362012587621280, 4.338193544061892837 ) ) ;
#13200 = CARTESIAN_POINT ( 'NONE',  ( 0.000000000000000000, 0.000000000000000000, 0.000000000000000000 ) ) ;
#13201 = CYLINDRICAL_SURFACE ( 'NONE', #5979, 15.00000000000000000 ) ;
#13202 = CARTESIAN_POINT ( 'NONE',  ( -45.43829269268871229, 413.5573905683720000, -3.332260488124726194 ) ) ;
#13203 = DIRECTION ( 'NONE',  ( 1.000000000000000000, 1.250996701150283068E-16, -0.000000000000000000 ) ) ;
#13204 = ORIENTED_EDGE ( 'NONE', *, *, #12757, .F. ) ;
#13205 = CARTESIAN_POINT ( 'NONE',  ( -42.82802356641966668, 425.9948905601784759, -14.14213562373094746 ) ) ;
#13206 = ADVANCED_FACE ( 'NONE', ( #9216 ), #2850, .F. ) ;
#13207 = ORIENTED_EDGE ( 'NONE', *, *, #11450, .F. ) ;
#13208 = CARTESIAN_POINT ( 'NONE',  ( -28.68588794268872633, 378.8848358243226357, 0.000000000000000000 ) ) ;
#13209 = ORIENTED_EDGE ( 'NONE', *, *, #20244, .T. ) ;
#13210 = ORIENTED_EDGE ( 'NONE', *, *, #9030, .T. ) ;
#13211 = DIRECTION ( 'NONE',  ( -0.000000000000000000, 1.000000000000000000, -0.000000000000000000 ) ) ;
#13212 = CARTESIAN_POINT ( 'NONE',  ( -47.16347859291443712, 306.6198905601784759, -7.653668647301793193 ) ) ;
#13213 = DIRECTION ( 'NONE',  ( 1.000000000000000000, 0.000000000000000000, 0.000000000000000000 ) ) ;
#13214 = CARTESIAN_POINT ( 'NONE',  ( -25.35362745456398059, 348.1823905683720000, 16.75240474999998952 ) ) ;
#13215 = CARTESIAN_POINT ( 'NONE',  ( -21.03221929538694113, 488.8698905765655809, -18.47759065022572855 ) ) ;
#13216 = CARTESIAN_POINT ( 'NONE',  ( -42.88789093042843348, 364.8073905683720568, 9.489475012073736337 ) ) ;
#13217 = CYLINDRICAL_SURFACE ( 'NONE', #8224, 20.57735571454641033 ) ;
#13218 = CARTESIAN_POINT ( 'NONE',  ( -19.19641293061498288, 387.3073905683720000, 14.20200298773971426 ) ) ;
#13219 = CARTESIAN_POINT ( 'NONE',  ( -14.54375231895776288, 298.2448905765656377, -14.14213562373094746 ) ) ;
#13220 = DIRECTION ( 'NONE',  ( -0.000000000000000000, -1.000000000000000000, 0.000000000000000000 ) ) ;
#13221 = CARTESIAN_POINT ( 'NONE',  ( -28.68588794268870501, 281.3698905683720000, -16.75240474999999307 ) ) ;
#13222 = DIRECTION ( 'NONE',  ( -1.191790137725560488E-16, 1.000000000000000000, -0.000000000000000000 ) ) ;
#13223 = CIRCLE ( 'NONE', #12540, 4.000000000000001776 ) ;
#13224 = CARTESIAN_POINT ( 'NONE',  ( -19.19641293061498999, 428.8073905683720000, 14.20200298773971426 ) ) ;
#13225 = LINE ( 'NONE', #6286, #17524 ) ;
#13226 = DIRECTION ( 'NONE',  ( -1.000000000000000000, 0.000000000000000000, 0.000000000000000000 ) ) ;
#13227 = CARTESIAN_POINT ( 'NONE',  ( -28.68588794268872277, 449.7448905601784759, 19.99999999999999289 ) ) ;
#13228 = B_SPLINE_CURVE_WITH_KNOTS ( 'NONE', 3,
 ( #15068, #9959, #19697, #8225, #9744, #13335 ),
 .UNSPECIFIED., .F., .F.,
 ( 4, 2, 4 ),
 ( 0.01067228060976418286, 0.01257272967502433454, 0.01447317874028448623 ),
 .UNSPECIFIED. ) ;
#13229 = CARTESIAN_POINT ( 'NONE',  ( -25.35362745456398059, 358.1823905683720000, 16.75240474999998952 ) ) ;
#13230 = CARTESIAN_POINT ( 'NONE',  ( -22.27502019258949062, 476.9948905683720000, 15.47720386886985189 ) ) ;
#13231 = ORIENTED_EDGE ( 'NONE', *, *, #3594, .T. ) ;
#13232 = CARTESIAN_POINT ( 'NONE',  ( -40.01497788969915348, 485.6823905601785327, -16.95518130045146421 ) ) ;
#13233 = CARTESIAN_POINT ( 'NONE',  ( -28.68588794268870501, 296.3698905683720568, 16.75240474999999307 ) ) ;
#13234 = ORIENTED_EDGE ( 'NONE', *, *, #20859, .F. ) ;
#13235 = DIRECTION ( 'NONE',  ( 1.000000000000000000, 0.000000000000000000, -0.000000000000000000 ) ) ;
#13236 = VERTEX_POINT ( 'NONE', #6075 ) ;
#13237 = LINE ( 'NONE', #11604, #1199 ) ;
#13238 = VECTOR ( 'NONE', #17527, 1000.000000000000000 ) ;
#13239 = CARTESIAN_POINT ( 'NONE',  ( -44.16309181155857289, 395.9948905683720568, 6.410867750099241924 ) ) ;
#13240 = CARTESIAN_POINT ( 'NONE',  ( -48.68588794268877251, 442.3073905765656377, 3.978247347593061978 ) ) ;
#13241 = CARTESIAN_POINT ( 'NONE',  ( 20.42502041961815351, 163.4113008177049551, 60.00000000000000000 ) ) ;
#13242 = CARTESIAN_POINT ( 'NONE',  ( -35.09675569278795138, 431.9948905683720568, -15.47720386886985544 ) ) ;
#13243 = CARTESIAN_POINT ( 'NONE',  ( -11.93348319268872970, 438.8698905683720568, -2.051577885510841163E-15 ) ) ;
#13244 = ITEM_DEFINED_TRANSFORMATION ( 'NONE', 'NONE', #3129,  #12794 ) ;
#13245 = CARTESIAN_POINT ( 'NONE',  ( -36.33955658999052218, 399.1198905601784759, 18.47759065022572500 ) ) ;
#13246 = CARTESIAN_POINT ( 'NONE',  ( -47.16347859291444422, 371.3698905765655809, -7.653668647301793193 ) ) ;
#13247 = DIRECTION ( 'NONE',  ( -1.000000000000000000, 0.000000000000000000, 0.000000000000000000 ) ) ;
#13248 = CARTESIAN_POINT ( 'NONE',  ( -21.03221929538691271, 264.1198905601784759, -18.47759065022572855 ) ) ;
#13249 = DIRECTION ( 'NONE',  ( 0.000000000000000000, -1.000000000000000000, 0.000000000000000000 ) ) ;
#13250 = DIRECTION ( 'NONE',  ( 0.000000000000000000, 0.000000000000000000, 1.000000000000000000 ) ) ;
#13251 = CARTESIAN_POINT ( 'NONE',  ( -38.17536295476246977, 493.8073905683720000, -14.20200298773971426 ) ) ;
#13252 = EDGE_CURVE ( 'NONE', #15047, #6356, #14532, .T. ) ;
#13253 = CIRCLE ( 'NONE', #20502, 4.000000000000000000 ) ;
#13254 = LINE ( 'NONE', #5017, #3354 ) ;
#13255 = DIRECTION ( 'NONE',  ( 0.000000000000000000, 1.000000000000000000, 0.000000000000000000 ) ) ;
#13256 = AXIS2_PLACEMENT_3D ( 'NONE', #1045, #14241, #14350 ) ;
#13257 = CARTESIAN_POINT ( 'NONE',  ( -11.93348319268872615, 400.0573905683720568, 3.332260488124728415 ) ) ;
#13258 = CYLINDRICAL_SURFACE ( 'NONE', #6793, 49.60091809715359545 ) ;
#13259 = EDGE_CURVE ( 'NONE', #8266, #9067, #14328, .T. ) ;
#13260 = CARTESIAN_POINT ( 'NONE',  ( -44.16309181155855867, 234.7448905683720000, -6.410867750099231266 ) ) ;
#13261 = CARTESIAN_POINT ( 'NONE',  ( -45.43829269268871229, 353.8698905683720568, 0.000000000000000000 ) ) ;
#13262 = ORIENTED_EDGE ( 'NONE', *, *, #595, .T. ) ;
#13263 = CARTESIAN_POINT ( 'NONE',  ( -32.01814843081346851, 526.0573905683720568, 16.75240474999999307 ) ) ;
#13264 = ORIENTED_EDGE ( 'NONE', *, *, #17251, .T. ) ;
#13265 = CARTESIAN_POINT ( 'NONE',  ( -22.27502019258949773, 442.2448905683720000, -15.47720386886985544 ) ) ;
#13266 = CARTESIAN_POINT ( 'NONE',  ( -14.48388495494901740, 519.8073905683720568, -9.489475012073736337 ) ) ;
#13267 = VERTEX_POINT ( 'NONE', #9110 ) ;
#13268 = CARTESIAN_POINT ( 'NONE',  ( -8.685887942688720997, 342.2448905601784759, -2.449293598294705724E-15 ) ) ;
#13269 = CARTESIAN_POINT ( 'NONE',  ( -11.93348319268873681, 489.1823905683720568, -3.332260488124732856 ) ) ;
#13270 = CIRCLE ( 'NONE', #18776, 5.000000000000004441 ) ;
#13271 = ORIENTED_EDGE ( 'NONE', *, *, #4990, .F. ) ;
#13272 = CARTESIAN_POINT ( 'NONE',  ( -11.93348319268873858, 498.5573905683720568, 3.332260488124728859 ) ) ;
#13273 = CARTESIAN_POINT ( 'NONE',  ( -28.68588794268872633, 489.7448905601784759, 19.99999999999999289 ) ) ;
#13274 = VECTOR ( 'NONE', #7326, 1000.000000000000000 ) ;
#13275 = CARTESIAN_POINT ( 'NONE',  ( -40.01497788969914637, 453.5573905765656377, 16.95518130045146776 ) ) ;
#13276 = DIRECTION ( 'NONE',  ( 0.000000000000000000, 0.000000000000000000, 1.000000000000000000 ) ) ;
#13277 = CARTESIAN_POINT ( 'NONE',  ( 147.4234352242185935, 620.7448905601785327, 1.893624729818134345 ) ) ;
#13278 = DIRECTION ( 'NONE',  ( 0.000000000000000000, 0.000000000000000000, 1.000000000000000000 ) ) ;
#13279 = LINE ( 'NONE', #10220, #14616 ) ;
#13280 = FACE_OUTER_BOUND ( 'NONE', #10358, .T. ) ;
#13281 = ADVANCED_FACE ( 'NONE', ( #15732 ), #918, .T. ) ;
#13282 = EDGE_CURVE ( 'NONE', #16900, #3036, #18514, .T. ) ;
#13283 = CARTESIAN_POINT ( 'NONE',  ( -45.64106924314019409, 492.9323905765655809, 11.32908994701042538 ) ) ;
#13284 = CARTESIAN_POINT ( 'NONE',  ( -35.09675569278794427, 307.2448905683720000, 15.47720386886985366 ) ) ;
#13285 = CARTESIAN_POINT ( 'NONE',  ( -24.70764059509556887, 530.0573905601785327, 19.99999999999998934 ) ) ;
#13286 = CARTESIAN_POINT ( 'NONE',  ( -24.70764059509553690, 270.0573905601784759, 19.99999999999998934 ) ) ;
#13287 = CARTESIAN_POINT ( 'NONE',  ( -10.20829729246299244, 416.3698905765656377, 7.653668647301790529 ) ) ;
#13288 = AXIS2_PLACEMENT_3D ( 'NONE', #15182, #8880, #16802 ) ;
#13289 = CARTESIAN_POINT ( 'NONE',  ( -19.19641293061497933, 291.9323905683720568, -14.20200298773971603 ) ) ;
#13290 = CARTESIAN_POINT ( 'NONE',  ( -32.01814843081346140, 507.5573905683720000, 16.75240474999999307 ) ) ;
#13291 = EDGE_CURVE ( 'NONE', #1447, #15711, #9533, .T. ) ;
#13292 = ORIENTED_EDGE ( 'NONE', *, *, #6180, .F. ) ;
#13293 = CARTESIAN_POINT ( 'NONE',  ( -32.01814843081346140, 467.5573905683721136, 16.75240474999999307 ) ) ;
#13294 = DIRECTION ( 'NONE',  ( 0.000000000000000000, 0.000000000000000000, 1.000000000000000000 ) ) ;
#13295 = CARTESIAN_POINT ( 'NONE',  ( -32.01814843081343298, 271.6823905683720000, -16.75240474999999307 ) ) ;
#13296 = ORIENTED_EDGE ( 'NONE', *, *, #12118, .T. ) ;
#13297 = CARTESIAN_POINT ( 'NONE',  ( 21.30000000000000071, 0.000000000000000000, 0.000000000000000000 ) ) ;
#13298 = CARTESIAN_POINT ( 'NONE',  ( -32.01814843081343298, 273.1823905683720000, -16.75240474999999307 ) ) ;
#13299 = CARTESIAN_POINT ( 'NONE',  ( -28.68588794268869790, 257.8698905683720000, 16.75240474999999307 ) ) ;
#13300 = EDGE_CURVE ( 'NONE', #16828, #20009, #15941, .T. ) ;
#13301 = CARTESIAN_POINT ( 'NONE',  ( -28.68588794268870146, 249.4948905765656093, -19.99999999999999289 ) ) ;
#13302 = CARTESIAN_POINT ( 'NONE',  ( 0.000000000000000000, 10.52886280891152104, 0.000000000000000000 ) ) ;
#13303 = CARTESIAN_POINT ( 'NONE',  ( -48.68588794268869435, 237.5573905601785043, 3.978247347593168115 ) ) ;
#13304 = CARTESIAN_POINT ( 'NONE',  ( -54.57497958038185004, 160.1716627696692683, 49.99999999999999289 ) ) ;
#13305 = CARTESIAN_POINT ( 'NONE',  ( -32.01814843081344009, 276.0573905683720000, 16.75240474999999307 ) ) ;
#13306 = CARTESIAN_POINT ( 'NONE',  ( -38.17536295476244845, 366.9323905683721136, 14.20200298773971781 ) ) ;
#13307 = CARTESIAN_POINT ( 'NONE',  ( -40.01497788969912506, 278.8073905601785327, 16.95518130045146776 ) ) ;
#13308 = CARTESIAN_POINT ( 'NONE',  ( -14.54375231895778242, 458.2448905765656377, -14.14213562373094746 ) ) ;
#13309 = CARTESIAN_POINT ( 'NONE',  ( -44.16309181155857999, 423.2448905683720568, -6.410867750099231266 ) ) ;
#13310 = CARTESIAN_POINT ( 'NONE',  ( -17.35679799567829207, 338.5573905765655809, -16.95518130045146421 ) ) ;
#13311 = ORIENTED_EDGE ( 'NONE', *, *, #13196, .T. ) ;
#13312 =( BOUNDED_CURVE ( )  B_SPLINE_CURVE ( 2, ( #6330, #16621, #19964, #6862, #6647, #13481, #9997, #1811, #19854, #11632, #81, #403, #18227, #507, #20074, #8589, #5143 ),
 .UNSPECIFIED., .F., .T. ) 
 B_SPLINE_CURVE_WITH_KNOTS ( ( 3, 2, 2, 2, 2, 2, 2, 2, 3 ),
 ( 0.3281250000000001110, 0.3300781250000001110, 0.3320312500000001110, 0.3339843750000001110, 0.3359375000000001110, 0.3378906250000001110, 0.3398437500000001110, 0.3417968750000001110, 0.3437500000000001110 ),
 .UNSPECIFIED. ) 
 CURVE ( )  GEOMETRIC_REPRESENTATION_ITEM ( )  RATIONAL_B_SPLINE_CURVE ( ( 0.9999999999999988898, 0.9807852804032315408, 1.000000000000000000, 0.9807852804032304306, 1.000000000000000000, 0.9807852804032304306, 1.000000000000000000, 0.9807852804032304306, 1.000000000000000000, 0.9807852804032304306, 1.000000000000000000, 0.9807852804032304306, 1.000000000000000000, 0.9807852804032304306, 1.000000000000000000, 0.9807852804032293204, 1.000000000000001110 ) ) 
 REPRESENTATION_ITEM ( '' )  );
#13313 = CARTESIAN_POINT ( 'NONE',  ( -36.33955658999052218, 419.1198905601784759, 18.47759065022572500 ) ) ;
#13314 = VERTEX_POINT ( 'NONE', #19281 ) ;
#13315 = DIRECTION ( 'NONE',  ( 1.000000000000000000, 0.000000000000000000, 0.000000000000000000 ) ) ;
#13316 = VERTEX_POINT ( 'NONE', #4463 ) ;
#13317 = ORIENTED_EDGE ( 'NONE', *, *, #14529, .F. ) ;
#13318 = CARTESIAN_POINT ( 'NONE',  ( -45.43829269268872650, 525.0573905683720568, -3.332260488124726194 ) ) ;
#13319 = CARTESIAN_POINT ( 'NONE',  ( -32.66413529028186957, 315.0573905601784190, -19.99999999999999289 ) ) ;
#13320 = DIRECTION ( 'NONE',  ( -1.000000000000000000, 0.000000000000000000, -0.000000000000000000 ) ) ;
#13321 = CARTESIAN_POINT ( 'NONE',  ( -14.48388495494899786, 341.3073905683721136, -9.489475012073734561 ) ) ;
#13322 = ORIENTED_EDGE ( 'NONE', *, *, #6364, .T. ) ;
#13323 = CARTESIAN_POINT ( 'NONE',  ( -21.03221929538692336, 485.1198905765656377, 18.47759065022572500 ) ) ;
#13324 = CARTESIAN_POINT ( 'NONE',  ( -22.27502019258947641, 366.9948905683720568, 15.47720386886985189 ) ) ;
#13325 =( REPRESENTATION_RELATIONSHIP ('NONE','NONE', #1888, #4076 ) REPRESENTATION_RELATIONSHIP_WITH_TRANSFORMATION ( #1016 )SHAPE_REPRESENTATION_RELATIONSHIP( ) );
#13326 = CARTESIAN_POINT ( 'NONE',  ( -32.01814843081344719, 371.6823905683720000, -16.75240474999999307 ) ) ;
#13327 = CARTESIAN_POINT ( 'NONE',  ( -10.20829729246297823, 306.3698905765655809, 7.653668647301790529 ) ) ;
#13328 = CARTESIAN_POINT ( 'NONE',  ( 158.8141120573112630, 610.7448905601785327, 0.000000000000000000 ) ) ;
#13329 = CARTESIAN_POINT ( 'NONE',  ( -13.20868407381884779, 259.4948905683720568, -6.410867750099233042 ) ) ;
#13330 = DIRECTION ( 'NONE',  ( -1.000000000000000000, 0.000000000000000000, 0.000000000000000000 ) ) ;
#13331 = EDGE_CURVE ( 'NONE', #10315, #18480, #20953, .T. ) ;
#13332 = CARTESIAN_POINT ( 'NONE',  ( -44.16309181155857999, 444.7448905683720000, -6.410867750099231266 ) ) ;
#13333 = ADVANCED_FACE ( 'NONE', ( #7904 ), #21116, .T. ) ;
#13334 = CARTESIAN_POINT ( 'NONE',  ( 20.42502041961813575, 271.1055109169419666, 40.00000000000000000 ) ) ;
#13335 = CARTESIAN_POINT ( 'NONE',  ( 0.5805565836007611225, 3.752776749732563477, 6.500000000000000000 ) ) ;
#13336 = CARTESIAN_POINT ( 'NONE',  ( 3.458603197740078627, 326.0737056351150613, -33.59072564020503648 ) ) ;
#13337 = DIRECTION ( 'NONE',  ( 0.000000000000000000, 0.000000000000000000, -1.000000000000000000 ) ) ;
#13338 = CARTESIAN_POINT ( 'NONE',  ( -38.17536295476245556, 343.8073905683720000, -14.20200298773971426 ) ) ;
#13339 = CARTESIAN_POINT ( 'NONE',  ( -22.27502019258949773, 480.7448905683720568, -15.47720386886985544 ) ) ;
#13340 = ORIENTED_EDGE ( 'NONE', *, *, #5421, .F. ) ;
#13341 = CARTESIAN_POINT ( 'NONE',  ( -8.685887942688736985, 492.2448905601785327, -2.449293598294705724E-15 ) ) ;
#13342 = CARTESIAN_POINT ( 'NONE',  ( -32.01814843081344009, 306.0573905683720000, 16.75240474999999307 ) ) ;
#13343 = DIRECTION ( 'NONE',  ( 1.000000000000000000, 9.855701800883827197E-17, -0.000000000000000000 ) ) ;
#13344 = VERTEX_POINT ( 'NONE', #3166 ) ;
#13345 = DIRECTION ( 'NONE',  ( -0.000000000000000000, -0.000000000000000000, 1.000000000000000000 ) ) ;
#13346 = CARTESIAN_POINT ( 'NONE',  ( -16.84014894278199748, 411.6198905683720568, -11.84573899990672707 ) ) ;
#13347 = CARTESIAN_POINT ( 'NONE',  ( -40.01497788969913927, 375.6823905601784190, -16.95518130045146421 ) ) ;
#13348 = CARTESIAN_POINT ( 'NONE',  ( -16.84014894278199748, 430.1198905683720000, -11.84573899990672707 ) ) ;
#13349 = CARTESIAN_POINT ( 'NONE',  ( -38.17536295476244135, 263.8073905683720568, -14.20200298773971426 ) ) ;
#13350 = CARTESIAN_POINT ( 'NONE',  ( -19.19641293061498999, 437.3073905683720568, 14.20200298773971426 ) ) ;
#13351 = APPLICATION_PROTOCOL_DEFINITION ( 'draft international standard', 'automotive_design', 1998, #2389 ) ;
#13352 = CYLINDRICAL_SURFACE ( 'NONE', #19008, 43.46661168214937732 ) ;
#13353 = CARTESIAN_POINT ( 'NONE',  ( -8.685887942688724550, 366.9948905765655809, -2.449293598294705724E-15 ) ) ;
#13354 = LINE ( 'NONE', #19943, #13789 ) ;
#13355 = PLANE ( 'NONE',  #16153 ) ;
#13356 = DIRECTION ( 'NONE',  ( 0.000000000000000000, 0.000000000000000000, 1.000000000000000000 ) ) ;
#13357 = DIRECTION ( 'NONE',  ( -1.191790137725560488E-16, 1.000000000000000000, -0.000000000000000000 ) ) ;
#13358 = CARTESIAN_POINT ( 'NONE',  ( -40.53162694259545873, 506.6198905683721136, 11.84573899990672885 ) ) ;
#13359 = DIRECTION ( 'NONE',  ( 1.191790137725560488E-16, -1.000000000000000000, -0.000000000000000000 ) ) ;
#13360 = CARTESIAN_POINT ( 'NONE',  ( -21.03221929538693402, 464.1198905601784759, -18.47759065022572855 ) ) ;
#13361 = CARTESIAN_POINT ( 'NONE',  ( -43.52372910701232911, 209.6355236139544331, 2.220491386914096754 ) ) ;
#13362 = VECTOR ( 'NONE', #16151, 1000.000000000000000 ) ;
#13363 = CARTESIAN_POINT ( 'NONE',  ( -38.17536295476246266, 413.8073905683719431, -14.20200298773971426 ) ) ;
#13364 = DIRECTION ( 'NONE',  ( 1.191790137725560488E-16, -1.000000000000000000, -0.000000000000000000 ) ) ;
#13365 = CARTESIAN_POINT ( 'NONE',  ( -13.20868407381884602, 230.9948905683720284, -6.410867750099233042 ) ) ;
#13366 = CARTESIAN_POINT ( 'NONE',  ( -35.09675569278794427, 371.9948905683720568, -15.47720386886985544 ) ) ;
#13367 = VECTOR ( 'NONE', #16639, 1000.000000000000000 ) ;
#13368 = VERTEX_POINT ( 'NONE', #8226 ) ;
#13369 = CARTESIAN_POINT ( 'NONE',  ( -22.27502019258949417, 516.9948905683720568, 15.47720386886985189 ) ) ;
#13370 = VERTEX_POINT ( 'NONE', #4773 ) ;
#13371 = CARTESIAN_POINT ( 'NONE',  ( -38.17536295476246266, 443.8073905683720568, -14.20200298773971426 ) ) ;
#13372 = CARTESIAN_POINT ( 'NONE',  ( -28.68588794268872988, 516.3698905683720568, 16.75240474999999307 ) ) ;
#13373 = ORIENTED_EDGE ( 'NONE', *, *, #8116, .T. ) ;
#13374 = CARTESIAN_POINT ( 'NONE',  ( -21.03221929538694468, 528.8698905765656946, -18.47759065022572855 ) ) ;
#13375 = CARTESIAN_POINT ( 'NONE',  ( -28.68588794268873343, 491.3698905683720568, -16.75240474999999307 ) ) ;
#13376 = EDGE_LOOP ( 'NONE', ( #8020, #15261, #7887, #14233 ) ) ;
#13377 = CARTESIAN_POINT ( 'NONE',  ( -42.88789093042845479, 504.8073905683721136, 9.489475012073734561 ) ) ;
#13378 = CARTESIAN_POINT ( 'NONE',  ( -19.45117422794473683, 45.67224592879905742, -48.73435233020793333 ) ) ;
#13379 = VECTOR ( 'NONE', #8690, 1000.000000000000000 ) ;
#13380 = CARTESIAN_POINT ( 'NONE',  ( -48.68588794268871567, 421.9948905765656377, 0.000000000000000000 ) ) ;
#13381 = CARTESIAN_POINT ( 'NONE',  ( -24.70764059509555821, 359.1823905765655809, -19.99999999999999289 ) ) ;
#13382 = ADVANCED_FACE ( 'NONE', ( #11369 ), #579, .T. ) ;
#13383 = DIRECTION ( 'NONE',  ( 1.000000000000000000, 0.000000000000000000, 0.000000000000000000 ) ) ;
#13384 = FACE_OUTER_BOUND ( 'NONE', #18187, .T. ) ;
#13385 = PLANE ( 'NONE',  #21169 ) ;
#13386 = PLANE ( 'NONE',  #19478 ) ;
#13387 = VECTOR ( 'NONE', #2105, 999.9999999999998863 ) ;
#13388 = FILL_AREA_STYLE ('',( #414 ) ) ;
#13389 = CARTESIAN_POINT ( 'NONE',  ( -42.82802356641967378, 493.2448905765656377, 14.14213562373094923 ) ) ;
#13390 = CARTESIAN_POINT ( 'NONE',  ( -13.20868407381884957, 289.7448905683720568, 6.410867750099229490 ) ) ;
#13391 = CARTESIAN_POINT ( 'NONE',  ( -24.70764059509554755, 234.4323905601785043, -19.99999999999999289 ) ) ;
#13392 = CARTESIAN_POINT ( 'NONE',  ( -11.73070664223723902, 273.1823905601784759, -11.32908994701042715 ) ) ;
#13393 = CARTESIAN_POINT ( 'NONE',  ( 158.8141120573112630, 620.7448905601785327, -4.999999999999990230 ) ) ;
#13394 = CARTESIAN_POINT ( 'NONE',  ( -38.17536295476244845, 283.8073905683720568, -14.20200298773971426 ) ) ;
#13395 = CIRCLE ( 'NONE', #6809, 4.000000000000001776 ) ;
#13396 = CARTESIAN_POINT ( 'NONE',  ( -14.54375231895779130, 533.4948905601785327, -14.14213562373094746 ) ) ;
#13397 = CARTESIAN_POINT ( 'NONE',  ( -22.27502019258949417, 508.4948905683720568, 15.47720386886985189 ) ) ;
#13398 = EDGE_CURVE ( 'NONE', #16131, #11348, #13003, .T. ) ;
#13399 = ORIENTED_EDGE ( 'NONE', *, *, #16446, .T. ) ;
#13400 = CARTESIAN_POINT ( 'NONE',  ( -44.16309181155857999, 465.9948905683720000, 6.410867750099241924 ) ) ;
#13401 = CARTESIAN_POINT ( 'NONE',  ( -45.64106924314018698, 411.0573905765655809, -11.32908994701042538 ) ) ;
#13402 = CARTESIAN_POINT ( 'NONE',  ( -42.88789093042841927, 262.9323905683720568, -9.489475012073736337 ) ) ;
#13403 = ORIENTED_EDGE ( 'NONE', *, *, #14210, .T. ) ;
#13404 = CARTESIAN_POINT ( 'NONE',  ( 0.000000000000000000, 0.000000000000000000, 4.000000000000000000 ) ) ;
#13405 = CARTESIAN_POINT ( 'NONE',  ( -38.17536295476244135, 243.8073905683720284, -14.20200298773971426 ) ) ;
#13406 = CARTESIAN_POINT ( 'NONE',  ( -17.35679799567827786, 245.4323905765656377, 16.95518130045146421 ) ) ;
#13407 = CARTESIAN_POINT ( 'NONE',  ( -24.70764059509554045, 310.0573905601784759, 19.99999999999998934 ) ) ;
#13408 = CARTESIAN_POINT ( 'NONE',  ( -48.68588794268869435, 236.9323905601785043, -3.978247347593158345 ) ) ;
#13409 = CARTESIAN_POINT ( 'NONE',  ( -40.53162694259542320, 265.1198905683720568, 11.84573899990672885 ) ) ;
#13410 = CARTESIAN_POINT ( 'NONE',  ( -13.20868407381885667, 349.7448905683720568, 6.410867750099229490 ) ) ;
#13411 = EDGE_CURVE ( 'NONE', #4398, #2785, #11263, .T. ) ;
#13412 = CARTESIAN_POINT ( 'NONE',  ( -28.68588794268870146, 279.7448905601784759, 19.99999999999999289 ) ) ;
#13413 = PLANE ( 'NONE',  #5213 ) ;
#13414 = CARTESIAN_POINT ( 'NONE',  ( -35.09675569278795848, 415.7448905683720000, 15.47720386886985366 ) ) ;
#13415 = FACE_OUTER_BOUND ( 'NONE', #3174, .T. ) ;
#13416 = ORIENTED_EDGE ( 'NONE', *, *, #13282, .F. ) ;
#13417 = CARTESIAN_POINT ( 'NONE',  ( -24.70764059509555466, 400.0573905601784759, 19.99999999999998934 ) ) ;
#13418 = ADVANCED_FACE ( 'NONE', ( #9745 ), #8335, .T. ) ;
#13419 = ORIENTED_EDGE ( 'NONE', *, *, #179, .F. ) ;
#13420 = ORIENTED_EDGE ( 'NONE', *, *, #8952, .T. ) ;
#13421 = VERTEX_POINT ( 'NONE', #9960 ) ;
#13422 = CARTESIAN_POINT ( 'NONE',  ( -13.20868407381888154, 530.9948905683720568, -6.410867750099233042 ) ) ;
#13423 = CARTESIAN_POINT ( 'NONE',  ( -14.54375231895776110, 293.4948905601785327, -14.14213562373094746 ) ) ;
#13424 = DIRECTION ( 'NONE',  ( 0.000000000000000000, 0.000000000000000000, 1.000000000000000000 ) ) ;
#13425 = CARTESIAN_POINT ( 'NONE',  ( -13.20868407381885490, 320.9948905683720568, -6.410867750099233042 ) ) ;
#13426 = ORIENTED_EDGE ( 'NONE', *, *, #6635, .F. ) ;
#13427 = CARTESIAN_POINT ( 'NONE',  ( -45.43829269268870519, 373.5573905683720568, -3.332260488124726194 ) ) ;
#13428 = CARTESIAN_POINT ( 'NONE',  ( -35.09675569278795138, 375.7448905683720000, 15.47720386886985366 ) ) ;
#13429 = CARTESIAN_POINT ( 'NONE',  ( -21.03221929538690205, 305.1198905765656377, 18.47759065022572500 ) ) ;
#13430 = DIRECTION ( 'NONE',  ( -1.000000000000000000, -0.000000000000000000, -0.000000000000000000 ) ) ;
#13431 = CARTESIAN_POINT ( 'NONE',  ( -38.17536295476243424, 265.4323905683721136, 14.20200298773971781 ) ) ;
#13432 = CARTESIAN_POINT ( 'NONE',  ( -11.73070664223725501, 441.3073905601785327, 11.32908994701042005 ) ) ;
#13433 = CARTESIAN_POINT ( 'NONE',  ( -32.01814843081345430, 423.1823905683720568, -16.75240474999999307 ) ) ;
#13434 = AXIS2_PLACEMENT_3D ( 'NONE', #9673, #9468, #1259 ) ;
#13435 = CARTESIAN_POINT ( 'NONE',  ( -32.65721457343089185, 51.69451264534966128, 120.6590201788547319 ) ) ;
#13436 = CARTESIAN_POINT ( 'NONE',  ( -17.35679799567830628, 500.6823905601784759, 16.95518130045146421 ) ) ;
#13437 = CARTESIAN_POINT ( 'NONE',  ( -24.70764059509554755, 360.0573905601785327, 19.99999999999998934 ) ) ;
#13438 = CARTESIAN_POINT ( 'NONE',  ( -48.68588794268871567, 407.2448905601784759, 0.000000000000000000 ) ) ;
#13439 = CARTESIAN_POINT ( 'NONE',  ( -16.84014894278198327, 319.1198905683720568, 11.84573899990672530 ) ) ;
#13440 = CARTESIAN_POINT ( 'NONE',  ( -11.93348319268873681, 488.5573905683720568, 3.332260488124728415 ) ) ;
#13441 = EDGE_LOOP ( 'NONE', ( #15154, #2220, #10768, #4552 ) ) ;
#13442 = CARTESIAN_POINT ( 'NONE',  ( -28.68588794268872988, 464.7448905601784759, -19.99999999999999289 ) ) ;
#13443 = CARTESIAN_POINT ( 'NONE',  ( -42.88789093042842637, 312.9323905683720000, -9.489475012073736337 ) ) ;
#13444 = ORIENTED_EDGE ( 'NONE', *, *, #7360, .F. ) ;
#13445 = CARTESIAN_POINT ( 'NONE',  ( 0.06682554136338024475, -4.993536075455418555, 4.350941807883115686 ) ) ;
#13446 = ORIENTED_EDGE ( 'NONE', *, *, #14360, .T. ) ;
#13447 = FACE_OUTER_BOUND ( 'NONE', #7738, .T. ) ;
#13448 = AXIS2_PLACEMENT_3D ( 'NONE', #1350, #16173, #9658 ) ;
#13449 = CARTESIAN_POINT ( 'NONE',  ( -11.93348319268872437, 390.3698905683720568, -2.051577885510841163E-15 ) ) ;
#13450 = CARTESIAN_POINT ( 'NONE',  ( -14.54375231895778064, 480.9948905601784759, 14.14213562373094568 ) ) ;
#13451 = DIRECTION ( 'NONE',  ( 0.000000000000000000, 1.000000000000000000, 0.000000000000000000 ) ) ;
#13452 = CARTESIAN_POINT ( 'NONE',  ( -11.93348319268872970, 428.5573905683720568, 3.332260488124728415 ) ) ;
#13453 = CARTESIAN_POINT ( 'NONE',  ( -14.48388495494898542, 251.3073905683720284, -9.489475012073736337 ) ) ;
#13454 = CARTESIAN_POINT ( 'NONE',  ( -13.20868407381886556, 418.2448905683720568, 6.410867750099229490 ) ) ;
#13455 = SHAPE_DEFINITION_REPRESENTATION ( #1666, #3392 ) ;
#13456 = DIRECTION ( 'NONE',  ( -1.191790137725560488E-16, 1.000000000000000000, -0.000000000000000000 ) ) ;
#13457 = CARTESIAN_POINT ( 'NONE',  ( -14.54375231895776999, 358.2448905765656377, -14.14213562373094746 ) ) ;
#13458 = DIRECTION ( 'NONE',  ( -0.000000000000000000, 0.000000000000000000, 1.000000000000000000 ) ) ;
#13459 = CARTESIAN_POINT ( 'NONE',  ( -48.68588794268871567, 391.9948905765656377, 0.000000000000000000 ) ) ;
#13460 = CARTESIAN_POINT ( 'NONE',  ( -22.27502019258947286, 326.9948905683720000, 15.47720386886985189 ) ) ;
#13461 = DIRECTION ( 'NONE',  ( -1.000000000000000000, -0.000000000000000000, -0.000000000000000000 ) ) ;
#13462 = CARTESIAN_POINT ( 'NONE',  ( -19.19641293061499709, 481.9323905683720000, -14.20200298773971603 ) ) ;
#13463 = ADVANCED_FACE ( 'NONE', ( #17963 ), #16579, .T. ) ;
#13464 = CARTESIAN_POINT ( 'NONE',  ( -36.33955658999052218, 433.8698905765655809, 18.47759065022572500 ) ) ;
#13465 = CARTESIAN_POINT ( 'NONE',  ( -8.685887942688742314, 573.2448905601785327, 2.449293598294706119E-15 ) ) ;
#13466 = CARTESIAN_POINT ( 'NONE',  ( -32.66413529028187668, 419.4323905601784190, 19.99999999999999289 ) ) ;
#13467 = EDGE_CURVE ( 'NONE', #2613, #15821, #4993, .T. ) ;
#13468 = AXIS2_PLACEMENT_3D ( 'NONE', #14739, #13220, #19808 ) ;
#13469 = EDGE_CURVE ( 'NONE', #10793, #11897, #7111, .T. ) ;
#13470 = CARTESIAN_POINT ( 'NONE',  ( -44.16309181155856578, 385.9948905683720568, 6.410867750099241924 ) ) ;
#13471 = LINE ( 'NONE', #18108, #15788 ) ;
#13472 = CARTESIAN_POINT ( 'NONE',  ( -32.01814843081343298, 223.1823905683720000, -16.75240474999999307 ) ) ;
#13473 = CARTESIAN_POINT ( 'NONE',  ( -28.68588794268871212, 366.3698905683720568, 16.75240474999999307 ) ) ;
#13474 = VERTEX_POINT ( 'NONE', #14642 ) ;
#13475 = CARTESIAN_POINT ( 'NONE',  ( -45.43829269268873361, 533.8698905683720568, 0.000000000000000000 ) ) ;
#13476 = ORIENTED_EDGE ( 'NONE', *, *, #18138, .T. ) ;
#13477 = CARTESIAN_POINT ( 'NONE',  ( -16.84014894278199748, 449.1198905683720568, 11.84573899990672530 ) ) ;
#13478 = CARTESIAN_POINT ( 'NONE',  ( -25.35362745456399836, 516.6823905683720568, 16.75240474999998952 ) ) ;
#13479 = ADVANCED_FACE ( 'NONE', ( #3272 ), #6718, .F. ) ;
#13480 = ORIENTED_EDGE ( 'NONE', *, *, #15894, .T. ) ;
#13481 = CARTESIAN_POINT ( 'NONE',  ( -17.35679799567829562, 430.6823905601785327, 16.95518130045146421 ) ) ;
#13482 = CARTESIAN_POINT ( 'NONE',  ( -38.17536295476246977, 482.3073905683720568, -14.20200298773971426 ) ) ;
#13483 = VERTEX_POINT ( 'NONE', #30 ) ;
#13484 = CARTESIAN_POINT ( 'NONE',  ( -38.17536295476246266, 495.4323905683719431, 14.20200298773971781 ) ) ;
#13485 = CARTESIAN_POINT ( 'NONE',  ( -48.68588794268882936, 487.5573905601784190, 3.978247347592901217 ) ) ;
#13486 = CARTESIAN_POINT ( 'NONE',  ( -10.20829729246299422, 426.3698905765656377, 7.653668647301790529 ) ) ;
#13487 = CARTESIAN_POINT ( 'NONE',  ( 151.4788465195079823, 620.7448905601785327, -8.917803138848077182 ) ) ;
#13488 = CARTESIAN_POINT ( 'NONE',  ( -17.35679799567828141, 248.5573905765656093, -16.95518130045146421 ) ) ;
#13489 = CARTESIAN_POINT ( 'NONE',  ( -48.68588794268871567, 407.2448905601784759, 0.000000000000000000 ) ) ;
#13490 = DIRECTION ( 'NONE',  ( 0.000000000000000000, 1.000000000000000000, 0.000000000000000000 ) ) ;
#13491 = CARTESIAN_POINT ( 'NONE',  ( 0.5805565836007702263, -7.505553499465148271, -1.692530754021427292E-16 ) ) ;
#13492 = FACE_OUTER_BOUND ( 'NONE', #8634, .T. ) ;
#13493 = CARTESIAN_POINT ( 'NONE',  ( -43.63268616469407846, 200.3053519615658615, -1.302651870180923099 ) ) ;
#13494 = VECTOR ( 'NONE', #12053, 1000.000000000000000 ) ;
#13495 = AXIS2_PLACEMENT_3D ( 'NONE', #16811, #4904, #18310 ) ;
#13496 = CARTESIAN_POINT ( 'NONE',  ( -38.17536295476244135, 296.9323905683720000, 14.20200298773971781 ) ) ;
#13497 = CARTESIAN_POINT ( 'NONE',  ( -28.68588794268873343, 529.7448905601785327, 19.99999999999999289 ) ) ;
#13498 = CARTESIAN_POINT ( 'NONE',  ( -48.68588794268869435, 267.2448905601784759, 0.000000000000000000 ) ) ;
#13499 = DIRECTION ( 'NONE',  ( 0.000000000000000000, 0.000000000000000000, 1.000000000000000000 ) ) ;
#13500 = CARTESIAN_POINT ( 'NONE',  ( -11.93348319268871371, 290.0573905683720000, 3.332260488124728415 ) ) ;
#13501 = ORIENTED_EDGE ( 'NONE', *, *, #7194, .T. ) ;
#13502 = DIRECTION ( 'NONE',  ( 0.000000000000000000, 1.000000000000000000, 0.000000000000000000 ) ) ;
#13503 = CARTESIAN_POINT ( 'NONE',  ( -45.43829269268872650, 495.6823905683720568, 3.332260488124734632 ) ) ;
#13504 = CIRCLE ( 'NONE', #1776, 15.00000000000000000 ) ;
#13505 = ORIENTED_EDGE ( 'NONE', *, *, #5775, .T. ) ;
#13506 = CARTESIAN_POINT ( 'NONE',  ( -45.43829269268871940, 465.6823905683720000, 3.332260488124734632 ) ) ;
#13507 = CARTESIAN_POINT ( 'NONE',  ( -17.35679799567830273, 408.5573905765656377, -16.95518130045146421 ) ) ;
#13508 = CARTESIAN_POINT ( 'NONE',  ( -22.27502019258946575, 266.9948905683720000, 15.47720386886985189 ) ) ;
#13509 = VECTOR ( 'NONE', #15398, 1000.000000000000114 ) ;
#13510 = ORIENTED_EDGE ( 'NONE', *, *, #5782, .F. ) ;
#13511 = CARTESIAN_POINT ( 'NONE',  ( -48.68588794268870856, 331.9948905765656377, 0.000000000000000000 ) ) ;
#13512 = CARTESIAN_POINT ( 'NONE',  ( -45.43829269268869808, 245.0573905683720000, -3.332260488124726638 ) ) ;
#13513 = AXIS2_PLACEMENT_3D ( 'NONE', #5591, #20739, #7527 ) ;
#13514 = CARTESIAN_POINT ( 'NONE',  ( -28.68588794268870146, 239.4948905765656377, -19.99999999999999289 ) ) ;
#13515 = AXIS2_PLACEMENT_3D ( 'NONE', #9656, #17985, #17879 ) ;
#13516 = CARTESIAN_POINT ( 'NONE',  ( -48.68588794268870856, 367.2448905601784759, 0.000000000000000000 ) ) ;
#13517 = CARTESIAN_POINT ( 'NONE',  ( -19.81321358049341086, 224.0162454934389586, -17.97266195050653437 ) ) ;
#13518 = CARTESIAN_POINT ( 'NONE',  ( -19.19641293061497223, 277.3073905683720000, 14.20200298773971426 ) ) ;
#13519 = CARTESIAN_POINT ( 'NONE',  ( -22.27502019258947641, 348.4948905683720000, 15.47720386886985189 ) ) ;
#13520 = EDGE_CURVE ( 'NONE', #661, #12347, #19594, .T. ) ;
#13521 = LINE ( 'NONE', #3561, #9244 ) ;
#13522 = VECTOR ( 'NONE', #1681, 1000.000000000000000 ) ;
#13523 = CARTESIAN_POINT ( 'NONE',  ( -11.93348319268872615, 399.1823905683720568, -3.332260488124732856 ) ) ;
#13524 = CARTESIAN_POINT ( 'NONE',  ( -45.64106924314020119, 508.1823905601784190, 11.32908994701042538 ) ) ;
#13525 = ORIENTED_EDGE ( 'NONE', *, *, #2353, .T. ) ;
#13526 = CIRCLE ( 'NONE', #5222, 15.00000000000000000 ) ;
#13527 = CARTESIAN_POINT ( 'NONE',  ( -32.66413529028188378, 405.0573905601784759, -19.99999999999999289 ) ) ;
#13528 = EDGE_LOOP ( 'NONE', ( #9365, #13264 ) ) ;
#13529 = LINE ( 'NONE', #1634, #11161 ) ;
#13530 = ORIENTED_EDGE ( 'NONE', *, *, #11701, .T. ) ;
#13531 = VERTEX_POINT ( 'NONE', #9641 ) ;
#13532 = CARTESIAN_POINT ( 'NONE',  ( -44.16309181155859420, 524.7448905683720568, -6.410867750099231266 ) ) ;
#13533 = CARTESIAN_POINT ( 'NONE',  ( -8.685887942688713892, 282.5573905601784759, -3.978247347593165895 ) ) ;
#13534 = CARTESIAN_POINT ( 'NONE',  ( -43.68320130047528238, 210.1357463702879613, -0.3279153920022768731 ) ) ;
#13535 = ORIENTED_EDGE ( 'NONE', *, *, #13921, .T. ) ;
#13536 = ADVANCED_FACE ( 'NONE', ( #1766 ), #4672, .T. ) ;
#13537 = CARTESIAN_POINT ( 'NONE',  ( -32.01814843081344009, 327.5573905683720568, 16.75240474999999307 ) ) ;
#13538 = ORIENTED_EDGE ( 'NONE', *, *, #5202, .T. ) ;
#13539 = CARTESIAN_POINT ( 'NONE',  ( -42.88789093042843348, 372.9323905683720568, -9.489475012073736337 ) ) ;
#13540 = CARTESIAN_POINT ( 'NONE',  ( -35.09675569278794427, 371.9948905683720568, -15.47720386886985544 ) ) ;
#13541 = CARTESIAN_POINT ( 'NONE',  ( -21.03221929538691626, 308.8698905765655809, -18.47759065022572855 ) ) ;
#13542 = CARTESIAN_POINT ( 'NONE',  ( -8.685887942688740537, 516.9948905765655809, -2.449293598294705724E-15 ) ) ;
#13543 = CARTESIAN_POINT ( 'NONE',  ( -44.16309181155855867, 274.4948905683720000, 6.410867750099241924 ) ) ;
#13544 = DIRECTION ( 'NONE',  ( -0.000000000000000000, -0.000000000000000000, 1.000000000000000000 ) ) ;
#13545 = CARTESIAN_POINT ( 'NONE',  ( -35.09675569278795848, 427.2448905683720568, 15.47720386886985366 ) ) ;
#13546 = EDGE_CURVE ( 'NONE', #8292, #7438, #6392, .T. ) ;
#13547 = FACE_BOUND ( 'NONE', #20769, .T. ) ;
#13548 = EDGE_CURVE ( 'NONE', #15417, #18006, #6497, .T. ) ;
#13549 = CARTESIAN_POINT ( 'NONE',  ( -45.64106924314019409, 451.0573905765656377, -11.32908994701042538 ) ) ;
#13550 = CARTESIAN_POINT ( 'NONE',  ( -17.35679799567827786, 275.4323905765655809, 16.95518130045146421 ) ) ;
#13551 = CARTESIAN_POINT ( 'NONE',  ( 5.299999999999999822, 0.000000000000000000, -4.400000000000000355 ) ) ;
#13552 = CARTESIAN_POINT ( 'NONE',  ( -28.68588794268870856, 337.8698905683720000, 16.75240474999999307 ) ) ;
#13553 = CARTESIAN_POINT ( 'NONE',  ( -16.84014894278199748, 457.6198905683720568, 11.84573899990672530 ) ) ;
#13554 = EDGE_LOOP ( 'NONE', ( #1398, #4737, #20891, #16270 ) ) ;
#13555=STYLED_ITEM('',(#21449),#4225);
#13556 = CARTESIAN_POINT ( 'NONE',  ( -48.68588794268872277, 467.5573905601785327, 3.978247347593168115 ) ) ;
#13557 = CARTESIAN_POINT ( 'NONE',  ( -44.16309181155855867, 294.4948905683720000, 6.410867750099241924 ) ) ;
#13558 = EDGE_LOOP ( 'NONE', ( #3121, #15394, #2350, #18055 ) ) ;
#13559 = CARTESIAN_POINT ( 'NONE',  ( 0.000000000000000000, 0.000000000000000000, 0.000000000000000000 ) ) ;
#13560 = VERTEX_POINT ( 'NONE', #13114 ) ;
#13561 = DIRECTION ( 'NONE',  ( -1.191790137725560488E-16, 1.000000000000000000, -0.000000000000000000 ) ) ;
#13562 = EDGE_CURVE ( 'NONE', #20822, #5825, #11317, .T. ) ;
#13563 = CARTESIAN_POINT ( 'NONE',  ( -11.93348319268872260, 380.0573905683720568, 3.332260488124728859 ) ) ;
#13564 = CARTESIAN_POINT ( 'NONE',  ( -28.68588794268874764, 575.7448905601785327, 0.000000000000000000 ) ) ;
#13565 = PRESENTATION_STYLE_ASSIGNMENT (( #14974 ) ) ;
#13566 = CARTESIAN_POINT ( 'NONE',  ( -32.01814843081345430, 426.0573905683720568, 16.75240474999999307 ) ) ;
#13567 = CARTESIAN_POINT ( 'NONE',  ( -44.16309181155855867, 264.7448905683720000, -6.410867750099231266 ) ) ;
#13568 = CARTESIAN_POINT ( 'NONE',  ( -45.43829269268871940, 433.8698905683720568, 0.000000000000000000 ) ) ;
#13569 = CARTESIAN_POINT ( 'NONE',  ( -48.68588794268871567, 397.2448905601784759, 0.000000000000000000 ) ) ;
#13570 = CARTESIAN_POINT ( 'NONE',  ( -40.01497788969913216, 363.5573905765656377, 16.95518130045146776 ) ) ;
#13571 = DIRECTION ( 'NONE',  ( -0.000000000000000000, 0.000000000000000000, -1.000000000000000000 ) ) ;
#13572 = CARTESIAN_POINT ( 'NONE',  ( -45.43829269268870519, 323.8698905683720000, 0.000000000000000000 ) ) ;
#13573 = LINE ( 'NONE', #14878, #6219 ) ;
#13574 = AXIS2_PLACEMENT_3D ( 'NONE', #16033, #7572, #20788 ) ;
#13575 =( BOUNDED_CURVE ( )  B_SPLINE_CURVE ( 2, ( #20390, #12603, #19195, #13912, #15644, #4050, #829, #612, #2229, #2333, #20501, #17152, #7177, #935, #14124, #14235, #2543 ),
 .UNSPECIFIED., .F., .T. ) 
 B_SPLINE_CURVE_WITH_KNOTS ( ( 3, 2, 2, 2, 2, 2, 2, 2, 3 ),
 ( 0.8906250000000002220, 0.8925781250000002220, 0.8945312500000002220, 0.8964843750000002220, 0.8984375000000002220, 0.9003906250000001110, 0.9023437500000001110, 0.9042968750000001110, 0.9062500000000001110 ),
 .UNSPECIFIED. ) 
 CURVE ( )  GEOMETRIC_REPRESENTATION_ITEM ( )  RATIONAL_B_SPLINE_CURVE ( ( 0.9999999999999977796, 0.9807852804032326510, 1.000000000000000000, 0.9807852804032304306, 1.000000000000000000, 0.9807852804032304306, 1.000000000000000000, 0.9807852804032304306, 1.000000000000000000, 0.9807852804032304306, 1.000000000000000000, 0.9807852804032304306, 1.000000000000000000, 0.9807852804032304306, 1.000000000000000000, 0.9807852804032293204, 1.000000000000001110 ) ) 
 REPRESENTATION_ITEM ( '' )  );
#13576 = CARTESIAN_POINT ( 'NONE',  ( -16.84014894278200103, 469.1198905683720568, 11.84573899990672530 ) ) ;
#13577 = CARTESIAN_POINT ( 'NONE',  ( 69.79185940953689737, 142.2976266388001250, -69.11456258820064136 ) ) ;
#13578 = CARTESIAN_POINT ( 'NONE',  ( 0.000000000000000000, 0.000000000000000000, 0.000000000000000000 ) ) ;
#13579 = CARTESIAN_POINT ( 'NONE',  ( -17.35679799567828852, 303.8073905601784759, -16.95518130045146421 ) ) ;
#13580 = CARTESIAN_POINT ( 'NONE',  ( -32.01814843081344719, 383.1823905683720568, -16.75240474999999307 ) ) ;
#13581 = CARTESIAN_POINT ( 'NONE',  ( -48.68588794268858777, 471.6823905765655240, -3.978247347593477201 ) ) ;
#13582 = AXIS2_PLACEMENT_3D ( 'NONE', #4718, #21270, #7953 ) ;
#13583 = CARTESIAN_POINT ( 'NONE',  ( -47.16347859291446554, 527.8698905601784190, 7.653668647301805628 ) ) ;
#13584 = CARTESIAN_POINT ( 'NONE',  ( -45.43829269268870519, 363.5573905683720568, -3.332260488124726194 ) ) ;
#13585 = ORIENTED_EDGE ( 'NONE', *, *, #7810, .T. ) ;
#13586 = CARTESIAN_POINT ( 'NONE',  ( -19.19641293061500420, 530.4323905683720568, -14.20200298773971603 ) ) ;
#13587 = VERTEX_POINT ( 'NONE', #16472 ) ;
#13588 = CARTESIAN_POINT ( 'NONE',  ( -36.33955658999050797, 355.3698905601784759, -18.47759065022572855 ) ) ;
#13589 = CARTESIAN_POINT ( 'NONE',  ( -28.68588794268873343, 526.3698905683720568, 16.75240474999999307 ) ) ;
#13590 = ORIENTED_EDGE ( 'NONE', *, *, #248, .T. ) ;
#13591 = CARTESIAN_POINT ( 'NONE',  ( -40.01497788969916058, 530.4323905765655809, -16.95518130045146421 ) ) ;
#13592 = CARTESIAN_POINT ( 'NONE',  ( -13.20868407381887266, 478.2448905683720568, 6.410867750099229490 ) ) ;
#13593 = ORIENTED_EDGE ( 'NONE', *, *, #2446, .T. ) ;
#13594 = CARTESIAN_POINT ( 'NONE',  ( -45.43829269268872650, 484.1823905683720568, 3.332260488124734632 ) ) ;
#13595 = CARTESIAN_POINT ( 'NONE',  ( -40.01497788969914637, 488.8073905601784759, 16.95518130045146776 ) ) ;
#13596 = CARTESIAN_POINT ( 'NONE',  ( -24.70764059509555821, 424.8073905765656377, 19.99999999999998934 ) ) ;
#13597 = CARTESIAN_POINT ( 'NONE',  ( -24.70764059509556176, 474.8073905765655809, 19.99999999999998934 ) ) ;
#13598 = CARTESIAN_POINT ( 'NONE',  ( -48.68588794268879383, 297.5573905601784759, 3.978247347592954952 ) ) ;
#13599 = CARTESIAN_POINT ( 'NONE',  ( -17.35679799567830628, 438.5573905765655809, -16.95518130045146421 ) ) ;
#13600 = CARTESIAN_POINT ( 'NONE',  ( 0.000000000000000000, 135.1716627696692683, 0.000000000000000000 ) ) ;
#13601=STYLED_ITEM('',(#21428),#19141);
#13602 = LINE ( 'NONE', #5575, #10730 ) ;
#13603 = CARTESIAN_POINT ( 'NONE',  ( -16.84014894278197971, 299.1198905683720000, 11.84573899990672530 ) ) ;
#13604 = EDGE_CURVE ( 'NONE', #19032, #2991, #3641, .T. ) ;
#13605 = CARTESIAN_POINT ( 'NONE',  ( -5.502341142637708238, 600.7448905601785327, 7.573322868991241741 ) ) ;
#13606 = CARTESIAN_POINT ( 'NONE',  ( -11.93348319268872970, 440.6823905683721136, -3.332260488124732856 ) ) ;
#13607 = CARTESIAN_POINT ( 'NONE',  ( 21.30000000000000071, 0.000000000000000000, 3.309499999999999886 ) ) ;
#13608 = CARTESIAN_POINT ( 'NONE',  ( -42.88789093042841927, 264.4323905683720568, -9.489475012073736337 ) ) ;
#13609 = CIRCLE ( 'NONE', #10817, 5.000000000000001776 ) ;
#13610 = VERTEX_POINT ( 'NONE', #14165 ) ;
#13611 = CARTESIAN_POINT ( 'NONE',  ( -162.2727221670389781, 30.52886280891152282, 0.000000000000000000 ) ) ;
#13612 = CARTESIAN_POINT ( 'NONE',  ( -11.93348319268873858, 500.3698905683720000, -2.051577885510841163E-15 ) ) ;
#13613 = AXIS2_PLACEMENT_3D ( 'NONE', #16361, #13544, #21323 ) ;
#13614 = VERTEX_POINT ( 'NONE', #866 ) ;
#13615 = CARTESIAN_POINT ( 'NONE',  ( -16.84014894278200458, 471.6198905683720000, -11.84573899990672707 ) ) ;
#13616 = FACE_OUTER_BOUND ( 'NONE', #10158, .T. ) ;
#13617 = CARTESIAN_POINT ( 'NONE',  ( -38.17536295476243424, 255.4323905683720284, 14.20200298773971781 ) ) ;
#13618 = ORIENTED_EDGE ( 'NONE', *, *, #5178, .F. ) ;
#13619 = CARTESIAN_POINT ( 'NONE',  ( -10.20829729246298356, 336.3698905765656377, 7.653668647301790529 ) ) ;
#13620 = DIRECTION ( 'NONE',  ( -0.000000000000000000, -0.000000000000000000, 1.000000000000000000 ) ) ;
#13621 = CARTESIAN_POINT ( 'NONE',  ( -25.35362745456397704, 242.5573905683720000, -16.75240474999999307 ) ) ;
#13622 = PLANE ( 'NONE',  #9308 ) ;
#13623 = CARTESIAN_POINT ( 'NONE',  ( -40.01497788969912506, 225.6823905601784759, -16.95518130045146421 ) ) ;
#13624 = CARTESIAN_POINT ( 'NONE',  ( 0.000000000000000000, 0.000000000000000000, 0.000000000000000000 ) ) ;
#13625 = CARTESIAN_POINT ( 'NONE',  ( -45.43829269268869808, 274.1823905683720000, 3.332260488124734632 ) ) ;
#13626 = AXIS2_PLACEMENT_3D ( 'NONE', #18479, #3456, #8312 ) ;
#13627 = CARTESIAN_POINT ( 'NONE',  ( -44.16309181155857289, 354.7448905683720568, -6.410867750099231266 ) ) ;
#13628 = LINE ( 'NONE', #2264, #5441 ) ;
#13629 =( BOUNDED_CURVE ( )  B_SPLINE_CURVE ( 2, ( #3843, #2127, #20604, #13803, #5779, #12384, #5569, #9024, #515, #7291, #6976, #18977, #7076, #4158, #20505, #13598, #18761 ),
 .UNSPECIFIED., .F., .T. ) 
 B_SPLINE_CURVE_WITH_KNOTS ( ( 3, 2, 2, 2, 2, 2, 2, 2, 3 ),
 ( 0.7343750000000003331, 0.7363281250000003331, 0.7382812500000002220, 0.7402343750000002220, 0.7421875000000002220, 0.7441406250000002220, 0.7460937500000002220, 0.7480468750000001110, 0.7500000000000001110 ),
 .UNSPECIFIED. ) 
 CURVE ( )  GEOMETRIC_REPRESENTATION_ITEM ( )  RATIONAL_B_SPLINE_CURVE ( ( 0.9999999999999966693, 0.9807852804032337612, 1.000000000000000000, 0.9807852804032304306, 1.000000000000000000, 0.9807852804032304306, 1.000000000000000000, 0.9807852804032304306, 1.000000000000000000, 0.9807852804032304306, 1.000000000000000000, 0.9807852804032304306, 1.000000000000000000, 0.9807852804032304306, 1.000000000000000000, 0.9807852804032293204, 1.000000000000001110 ) ) 
 REPRESENTATION_ITEM ( '' )  );
#13630 = CARTESIAN_POINT ( 'NONE',  ( -19.19641293061498999, 407.3073905683720000, 14.20200298773971426 ) ) ;
#13631 = CARTESIAN_POINT ( 'NONE',  ( -10.20829729246298356, 337.6198905765656377, -7.653668647301794969 ) ) ;
#13632 = CARTESIAN_POINT ( 'NONE',  ( -47.16347859291445133, 406.6198905601784759, -7.653668647301793193 ) ) ;
#13633 = VERTEX_POINT ( 'NONE', #20029 ) ;
#13634 = CYLINDRICAL_SURFACE ( 'NONE', #3573, 220.7252770684331438 ) ;
#13635 = VERTEX_POINT ( 'NONE', #8655 ) ;
#13636 = EDGE_LOOP ( 'NONE', ( #1917, #5138, #20466 ) ) ;
#13637 = CARTESIAN_POINT ( 'NONE',  ( -19.19641293061499709, 518.8073905683720568, 14.20200298773971426 ) ) ;
#13638 = CARTESIAN_POINT ( 'NONE',  ( -11.73070664223723725, 291.3073905601784759, 11.32908994701042005 ) ) ;
#13639 = CARTESIAN_POINT ( 'NONE',  ( -33.84809828339280102, 56.85652257517428865, -152.3753892284480003 ) ) ;
#13640 = ORIENTED_EDGE ( 'NONE', *, *, #6166, .F. ) ;
#13641 = CARTESIAN_POINT ( 'NONE',  ( -45.43829269268870519, 315.3698905683720568, 0.000000000000000000 ) ) ;
#13642 = EDGE_LOOP ( 'NONE', ( #19391, #5589, #1633, #12512 ) ) ;
#13643 = CARTESIAN_POINT ( 'NONE',  ( -45.43829269268871229, 343.8698905683720000, 0.000000000000000000 ) ) ;
#13644 = CARTESIAN_POINT ( 'NONE',  ( -14.48388495494899786, 357.9323905683720000, 9.489475012073731008 ) ) ;
#13645 = CARTESIAN_POINT ( 'NONE',  ( -36.33955658999050087, 310.1198905765656377, -18.47759065022572855 ) ) ;
#13646 = CARTESIAN_POINT ( 'NONE',  ( 6.416697501590670427, 217.7548513357008630, 45.00000000000000000 ) ) ;
#13647 = EDGE_CURVE ( 'NONE', #1235, #12168, #6662, .T. ) ;
#13648 = CARTESIAN_POINT ( 'NONE',  ( -28.68588794268870501, 271.3698905683720000, -16.75240474999999307 ) ) ;
#13649 = CARTESIAN_POINT ( 'NONE',  ( -43.47668584505345990, 200.8081422174835780, 2.511554223531089036 ) ) ;
#13650 = CARTESIAN_POINT ( 'NONE',  ( -45.43829269268871229, 415.6823905683721136, 3.332260488124734632 ) ) ;
#13651 = CARTESIAN_POINT ( 'NONE',  ( -23.81512245425836838, 45.39025379435859975, 122.7127025493173846 ) ) ;
#13652 = CARTESIAN_POINT ( 'NONE',  ( -32.66413529028189089, 504.1823905765656377, 19.99999999999999289 ) ) ;
#13653 = FACE_OUTER_BOUND ( 'NONE', #14116, .T. ) ;
#13654 = CARTESIAN_POINT ( 'NONE',  ( -38.17536295476244845, 336.9323905683720568, 14.20200298773971781 ) ) ;
#13655 = CARTESIAN_POINT ( 'NONE',  ( -45.43829269268871940, 463.5573905683720568, -3.332260488124726194 ) ) ;
#13656 = ORIENTED_EDGE ( 'NONE', *, *, #13998, .F. ) ;
#13657 = CARTESIAN_POINT ( 'NONE',  ( -32.66413529028189089, 469.4323905601784759, 19.99999999999999289 ) ) ;
#13658 = CARTESIAN_POINT ( 'NONE',  ( -11.93348319268871016, 278.8698905683720000, -2.051577885510841163E-15 ) ) ;
#13659 = CARTESIAN_POINT ( 'NONE',  ( 0.000000000000000000, 7.505553499465139389, 0.000000000000000000 ) ) ;
#13660 = ORIENTED_EDGE ( 'NONE', *, *, #7414, .T. ) ;
#13661 = LINE ( 'NONE', #13767, #15361 ) ;
#13662 = CARTESIAN_POINT ( 'NONE',  ( -24.70764059509554755, 340.0573905601784759, 19.99999999999998934 ) ) ;
#13663 = CARTESIAN_POINT ( 'NONE',  ( -35.09675569278793716, 301.9948905683720568, -15.47720386886985544 ) ) ;
#13664 = EDGE_CURVE ( 'NONE', #9092, #349, #8869, .T. ) ;
#13665 = CARTESIAN_POINT ( 'NONE',  ( -19.19641293061498644, 381.9323905683720000, -14.20200298773971603 ) ) ;
#13666 = CARTESIAN_POINT ( 'NONE',  ( -17.35679799567827430, 230.6823905601784759, 16.95518130045146421 ) ) ;
#13667 =( LENGTH_UNIT ( ) NAMED_UNIT ( * ) SI_UNIT ( .MILLI., .METRE. ) );
#13668 = CARTESIAN_POINT ( 'NONE',  ( -11.93348319268872793, 418.8698905683720568, -2.051577885510841163E-15 ) ) ;
#13669 = CARTESIAN_POINT ( 'NONE',  ( -11.93348319268871194, 270.6823905683719431, -3.332260488124732856 ) ) ;
#13670 = CARTESIAN_POINT ( 'NONE',  ( -45.43829269268871940, 434.1823905683721136, 3.332260488124734632 ) ) ;
#13671 = APPLICATION_PROTOCOL_DEFINITION ( 'draft international standard', 'automotive_design', 1998, #4184 ) ;
#13672 = CARTESIAN_POINT ( 'NONE',  ( -28.68588794268871212, 364.4948905765656377, 19.99999999999999289 ) ) ;
#13673 = CARTESIAN_POINT ( 'NONE',  ( -13.20868407381885490, 319.4948905683720000, -6.410867750099233042 ) ) ;
#13674 = CARTESIAN_POINT ( 'NONE',  ( -11.93348319268873503, 470.0573905683720568, 3.332260488124728415 ) ) ;
#13675 = LINE ( 'NONE', #3713, #12336 ) ;
#13676 = CARTESIAN_POINT ( 'NONE',  ( -43.15185836128297581, 202.0883771310975021, -3.971358459629989124 ) ) ;
#13677 = CARTESIAN_POINT ( 'NONE',  ( -48.68588794268853803, 306.9323905601784759, -3.978247347593583783 ) ) ;
#13678 = EDGE_CURVE ( 'NONE', #15898, #8381, #9275, .T. ) ;
#13679 = CARTESIAN_POINT ( 'NONE',  ( -28.68588794268871922, 382.8698905683720000, -16.75240474999999307 ) ) ;
#13680 = LINE ( 'NONE', #16929, #7482 ) ;
#13681 = CARTESIAN_POINT ( 'NONE',  ( -28.68588794268873698, 534.7448905601785327, -19.99999999999999289 ) ) ;
#13682 = CARTESIAN_POINT ( 'NONE',  ( -25.35362745456398059, 346.6823905683720568, 16.75240474999998952 ) ) ;
#13683 = ORIENTED_EDGE ( 'NONE', *, *, #595, .F. ) ;
#13684 = CARTESIAN_POINT ( 'NONE',  ( -13.20868407381887977, 528.2448905683720568, 6.410867750099229490 ) ) ;
#13685 = VERTEX_POINT ( 'NONE', #3585 ) ;
#13686 = CARTESIAN_POINT ( 'NONE',  ( -13.20868407381887977, 519.4948905683720568, -6.410867750099233042 ) ) ;
#13687 = CARTESIAN_POINT ( 'NONE',  ( 28.16023193154655502, 323.8848358243226357, 20.00000000000000355 ) ) ;
#13688 = EDGE_CURVE ( 'NONE', #11055, #232, #5839, .T. ) ;
#13689 = DIRECTION ( 'NONE',  ( 0.000000000000000000, 0.000000000000000000, -1.000000000000000000 ) ) ;
#13690 = CARTESIAN_POINT ( 'NONE',  ( -11.73070664223727100, 527.9323905765655809, -11.32908994701042538 ) ) ;
#13691 = CARTESIAN_POINT ( 'NONE',  ( -40.53162694259545162, 482.6198905683720000, -11.84573899990672707 ) ) ;
#13692 = ORIENTED_EDGE ( 'NONE', *, *, #7435, .F. ) ;
#13693 = CARTESIAN_POINT ( 'NONE',  ( -32.01814843081345430, 486.0573905683721136, 16.75240474999999307 ) ) ;
#13694 = CARTESIAN_POINT ( 'NONE',  ( -32.66413529028188378, 489.4323905601784759, 19.99999999999999289 ) ) ;
#13695 = CARTESIAN_POINT ( 'NONE',  ( -8.685887942688728103, 416.9948905765656377, -2.449293598294705724E-15 ) ) ;
#13696 = CARTESIAN_POINT ( 'NONE',  ( 51.98438129372387806, -133.1434774248255906, 117.7249735956185219 ) ) ;
#13697 = LINE ( 'NONE', #8917, #5416 ) ;
#13698 = DIRECTION ( 'NONE',  ( 0.000000000000000000, 0.000000000000000000, 1.000000000000000000 ) ) ;
#13699 = CARTESIAN_POINT ( 'NONE',  ( 115.7989814974898337, 142.5259582928263455, 20.00000000000000355 ) ) ;
#13700 = AXIS2_PLACEMENT_3D ( 'NONE', #9323, #19179, #2634 ) ;
#13701 = CARTESIAN_POINT ( 'NONE',  ( -48.68588794268873698, 548.2448905601784190, 0.000000000000000000 ) ) ;
#13702 = SURFACE_STYLE_USAGE ( .BOTH. , #10434 ) ;
#13703 = DIRECTION ( 'NONE',  ( -0.000000000000000000, -1.000000000000000000, -0.000000000000000000 ) ) ;
#13704 = CARTESIAN_POINT ( 'NONE',  ( -14.48388495494899253, 301.3073905683720568, -9.489475012073736337 ) ) ;
#13705 = AXIS2_PLACEMENT_3D ( 'NONE', #13605, #18559, #3742 ) ;
#13706 = LINE ( 'NONE', #1934, #21288 ) ;
#13707 = CARTESIAN_POINT ( 'NONE',  ( -25.35362745456400191, 442.5573905683720568, -16.75240474999999307 ) ) ;
#13708 = CARTESIAN_POINT ( 'NONE',  ( -32.66413529028187668, 399.8073905765656377, -19.99999999999999289 ) ) ;
#13709 = CARTESIAN_POINT ( 'NONE',  ( -40.53162694259543031, 274.1198905683720568, -11.84573899990672707 ) ) ;
#13710 = VERTEX_POINT ( 'NONE', #18029 ) ;
#13711 = DIRECTION ( 'NONE',  ( 1.000000000000000000, 0.000000000000000000, 0.000000000000000000 ) ) ;
#13712 = CARTESIAN_POINT ( 'NONE',  ( -11.93348319268873681, 490.6823905683720568, -3.332260488124732856 ) ) ;
#13713 = VECTOR ( 'NONE', #13364, 1000.000000000000000 ) ;
#13714 = VERTEX_POINT ( 'NONE', #8069 ) ;
#13715 = CARTESIAN_POINT ( 'NONE',  ( -32.01814843081346140, 473.1823905683720000, -16.75240474999999307 ) ) ;
#13716 = CYLINDRICAL_SURFACE ( 'NONE', #10371, 19.99999999999999645 ) ;
#13717 = CARTESIAN_POINT ( 'NONE',  ( -32.01814843081343298, 251.6823905683720568, -16.75240474999999307 ) ) ;
#13718 = EDGE_CURVE ( 'NONE', #1090, #1338, #19650, .T. ) ;
#13719 = ORIENTED_EDGE ( 'NONE', *, *, #5844, .F. ) ;
#13720 = CARTESIAN_POINT ( 'NONE',  ( -28.68588794268874054, 573.2448905601785327, 0.000000000000000000 ) ) ;
#13721 = ADVANCED_FACE ( 'NONE', ( #12957 ), #19546, .F. ) ;
#13722 = AXIS2_PLACEMENT_3D ( 'NONE', #11076, #9132, #15754 ) ;
#13723 = CARTESIAN_POINT ( 'NONE',  ( -14.54375231895778064, 475.7448905765655809, 14.14213562373094568 ) ) ;
#13724 = CARTESIAN_POINT ( 'NONE',  ( -28.68588794268871567, 389.7448905601785327, 19.99999999999999289 ) ) ;
#13725 = CARTESIAN_POINT ( 'NONE',  ( -16.84014894278197261, 249.1198905683720284, 11.84573899990672530 ) ) ;
#13726 = CARTESIAN_POINT ( 'NONE',  ( -28.68588794268872277, 419.4948905765656377, -19.99999999999999289 ) ) ;
#13727 = CARTESIAN_POINT ( 'NONE',  ( -32.66413529028186247, 235.0573905601785043, -19.99999999999999289 ) ) ;
#13728 = CARTESIAN_POINT ( 'NONE',  ( -28.68588794268869790, 256.3698905683720000, 16.75240474999999307 ) ) ;
#13729 = CARTESIAN_POINT ( 'NONE',  ( -25.35362745456398059, 358.1823905683720000, 16.75240474999998952 ) ) ;
#13730 = EDGE_CURVE ( 'NONE', #952, #10871, #16122, .T. ) ;
#13731 = CIRCLE ( 'NONE', #7502, 15.00000000000000000 ) ;
#13732 = CARTESIAN_POINT ( 'NONE',  ( -162.2727221670389781, 10.52886280891152104, 0.000000000000000000 ) ) ;
#13733 = APPLICATION_CONTEXT ( 'automotive_design' ) ;
#13734 = ADVANCED_FACE ( 'NONE', ( #3116 ), #14699, .T. ) ;
#13735 = EDGE_CURVE ( 'NONE', #1162, #5244, #4713, .T. ) ;
#13736 = VECTOR ( 'NONE', #10274, 1000.000000000000000 ) ;
#13737 = CARTESIAN_POINT ( 'NONE',  ( -28.68588794268871567, 396.3698905683720000, 16.75240474999999307 ) ) ;
#13738 = CARTESIAN_POINT ( 'NONE',  ( -32.66413529028189089, 509.4323905601784190, 19.99999999999999289 ) ) ;
#13739 = CARTESIAN_POINT ( 'NONE',  ( -40.01497788969913927, 408.8073905601784759, 16.95518130045146776 ) ) ;
#13740 = ORIENTED_EDGE ( 'NONE', *, *, #9485, .T. ) ;
#13741 = DIRECTION ( 'NONE',  ( -1.000000000000000000, 0.000000000000000000, 0.000000000000000000 ) ) ;
#13742 = VERTEX_POINT ( 'NONE', #19334 ) ;
#13743 = ORIENTED_EDGE ( 'NONE', *, *, #13688, .T. ) ;
#13744 = CARTESIAN_POINT ( 'NONE',  ( -38.17536295476246977, 526.9323905683719431, 14.20200298773971781 ) ) ;
#13745 = CARTESIAN_POINT ( 'NONE',  ( -42.82802356641965247, 285.9948905601784759, -14.14213562373094746 ) ) ;
#13746 = FACE_OUTER_BOUND ( 'NONE', #1547, .T. ) ;
#13747 = ADVANCED_FACE ( 'NONE', ( #9800 ), #16423, .F. ) ;
#13748 = CARTESIAN_POINT ( 'NONE',  ( -19.19641293061497578, 318.8073905683720568, 14.20200298773971426 ) ) ;
#13749 = VERTEX_POINT ( 'NONE', #7651 ) ;
#13750 = CARTESIAN_POINT ( 'NONE',  ( -25.35362745456399125, 351.0573905683720568, -16.75240474999999307 ) ) ;
#13751 = CARTESIAN_POINT ( 'NONE',  ( -25.35362745456398059, 356.6823905683720568, 16.75240474999998952 ) ) ;
#13752 = CARTESIAN_POINT ( 'NONE',  ( -28.68588794268870501, 279.4948905765656377, -19.99999999999999289 ) ) ;
#13753 = DIRECTION ( 'NONE',  ( -1.000000000000000000, 0.000000000000000000, 0.000000000000000000 ) ) ;
#13754 = CARTESIAN_POINT ( 'NONE',  ( -40.53162694259543031, 275.1198905683720568, 11.84573899990672885 ) ) ;
#13755 = FACE_OUTER_BOUND ( 'NONE', #572, .T. ) ;
#13756 =( BOUNDED_CURVE ( )  B_SPLINE_CURVE ( 2, ( #14351, #4591, #2767, #9557, #14454, #21247, #19618, #7824, #16176, #3188, #1249, #7926, #12819, #19410, #17885, #11185, #17787 ),
 .UNSPECIFIED., .F., .T. ) 
 B_SPLINE_CURVE_WITH_KNOTS ( ( 3, 2, 2, 2, 2, 2, 2, 2, 3 ),
 ( 0.8593750000000002220, 0.8613281250000002220, 0.8632812500000002220, 0.8652343750000002220, 0.8671875000000002220, 0.8691406250000002220, 0.8710937500000002220, 0.8730468750000002220, 0.8750000000000002220 ),
 .UNSPECIFIED. ) 
 CURVE ( )  GEOMETRIC_REPRESENTATION_ITEM ( )  RATIONAL_B_SPLINE_CURVE ( ( 0.9999999999999977796, 0.9807852804032326510, 1.000000000000000000, 0.9807852804032304306, 1.000000000000000000, 0.9807852804032304306, 1.000000000000000000, 0.9807852804032304306, 1.000000000000000000, 0.9807852804032304306, 1.000000000000000000, 0.9807852804032304306, 1.000000000000000000, 0.9807852804032304306, 1.000000000000000000, 0.9807852804032282101, 1.000000000000002220 ) ) 
 REPRESENTATION_ITEM ( '' )  );
#13757 = CARTESIAN_POINT ( 'NONE',  ( -19.19641293061498999, 408.8073905683720000, 14.20200298773971426 ) ) ;
#13758 = LINE ( 'NONE', #18290, #14096 ) ;
#13759 = CARTESIAN_POINT ( 'NONE',  ( -48.68588794268872277, 501.9948905765656377, 0.000000000000000000 ) ) ;
#13760 = CARTESIAN_POINT ( 'NONE',  ( -8.685887942688726326, 412.2448905601784759, -2.449293598294705724E-15 ) ) ;
#13761 = CARTESIAN_POINT ( 'NONE',  ( -14.48388495494899431, 329.4323905683720568, 9.489475012073732785 ) ) ;
#13762 = CARTESIAN_POINT ( 'NONE',  ( -22.27502019258948707, 456.9948905683720000, 15.47720386886985189 ) ) ;
#13763 = ORIENTED_EDGE ( 'NONE', *, *, #9152, .T. ) ;
#13764 = CARTESIAN_POINT ( 'NONE',  ( -8.685887942688736985, 472.5573905601784759, -3.978247347593165895 ) ) ;
#13765 = CARTESIAN_POINT ( 'NONE',  ( -16.84014894278198327, 290.1198905683720568, -11.84573899990672707 ) ) ;
#13766 = VERTEX_POINT ( 'NONE', #1184 ) ;
#13767 = CARTESIAN_POINT ( 'NONE',  ( -11.06088464903280233, 135.1716627696692683, 5.773301668816269938 ) ) ;
#13768 = CARTESIAN_POINT ( 'NONE',  ( -48.68588794268870856, 337.5573905601784759, 3.978247347593168115 ) ) ;
#13769 = CARTESIAN_POINT ( 'NONE',  ( -42.88789093042842637, 292.9323905683720568, -9.489475012073736337 ) ) ;
#13770 = CARTESIAN_POINT ( 'NONE',  ( -45.43829269268871229, 375.0573905683720000, -3.332260488124726638 ) ) ;
#13771 = CARTESIAN_POINT ( 'NONE',  ( -17.35679799567831694, 528.5573905765656946, -16.95518130045146421 ) ) ;
#13772 = CARTESIAN_POINT ( 'NONE',  ( -44.16309181155857999, 413.2448905683720568, -6.410867750099231266 ) ) ;
#13773 = CARTESIAN_POINT ( 'NONE',  ( -13.20868407381884779, 259.7448905683720000, 6.410867750099229490 ) ) ;
#13774 = CARTESIAN_POINT ( 'NONE',  ( -32.01814843081344719, 426.0573905683720568, 16.75240474999999307 ) ) ;
#13775 = ITEM_DEFINED_TRANSFORMATION ( 'NONE', 'NONE', #13851,  #12794 ) ;
#13776 = AXIS2_PLACEMENT_3D ( 'NONE', #11979, #9049, #11581 ) ;
#13777 = CARTESIAN_POINT ( 'NONE',  ( -32.66413529028187668, 334.1823905765656377, 19.99999999999999289 ) ) ;
#13778 = CARTESIAN_POINT ( 'NONE',  ( -21.03221929538691271, 274.1198905601784759, -18.47759065022572855 ) ) ;
#13779 = CARTESIAN_POINT ( 'NONE',  ( -25.35362745456398770, 331.0573905683720000, -16.75240474999999307 ) ) ;
#13780 = CARTESIAN_POINT ( 'NONE',  ( -38.17536295476246266, 476.9323905683720568, 14.20200298773971781 ) ) ;
#13781 = DIRECTION ( 'NONE',  ( -1.000000000000000000, 0.000000000000000000, 0.000000000000000000 ) ) ;
#13782 = CARTESIAN_POINT ( 'NONE',  ( -43.58160426315848213, 200.4655464737082013, -1.772246553899821997 ) ) ;
#13783 = LINE ( 'NONE', #16926, #2302 ) ;
#13784 = EDGE_CURVE ( 'NONE', #18441, #339, #20862, .T. ) ;
#13785 = CARTESIAN_POINT ( 'NONE',  ( -13.20868407381886023, 379.7448905683720000, 6.410867750099229490 ) ) ;
#13786 = CARTESIAN_POINT ( 'NONE',  ( -32.27528734226235230, 51.02792179363947156, -120.7615045227926771 ) ) ;
#13787 = CARTESIAN_POINT ( 'NONE',  ( -10.20829729246300488, 521.6198905601785327, 7.653668647301790529 ) ) ;
#13788 = CARTESIAN_POINT ( 'NONE',  ( -19.19641293061498288, 347.3073905683720568, 14.20200298773971426 ) ) ;
#13789 = VECTOR ( 'NONE', #20366, 1000.000000000000000 ) ;
#13790 = ORIENTED_EDGE ( 'NONE', *, *, #16330, .F. ) ;
#13791 = CARTESIAN_POINT ( 'NONE',  ( -25.35362745456400901, 501.0573905683720568, -16.75240474999999307 ) ) ;
#13792 = ORIENTED_EDGE ( 'NONE', *, *, #6044, .F. ) ;
#13793 = DIRECTION ( 'NONE',  ( -1.000000000000000000, -1.191790137725560488E-16, 0.000000000000000000 ) ) ;
#13794 = CARTESIAN_POINT ( 'NONE',  ( -28.68588794268870856, 314.7448905601785327, -19.99999999999999289 ) ) ;
#13795 = DIRECTION ( 'NONE',  ( 1.191790137725560488E-16, -1.000000000000000000, 0.000000000000000000 ) ) ;
#13796 = CARTESIAN_POINT ( 'NONE',  ( -32.01814843081346140, 461.6823905683720568, -16.75240474999999307 ) ) ;
#13797 = ORIENTED_EDGE ( 'NONE', *, *, #18469, .T. ) ;
#13798 = CARTESIAN_POINT ( 'NONE',  ( -40.53162694259545162, 485.1198905683720000, 11.84573899990672885 ) ) ;
#13799 = DIRECTION ( 'NONE',  ( -0.000000000000000000, -0.000000000000000000, -1.000000000000000000 ) ) ;
#13800 = EDGE_CURVE ( 'NONE', #13714, #9575, #9559, .T. ) ;
#13801 = CARTESIAN_POINT ( 'NONE',  ( -28.68588794268872277, 429.4948905765655809, -19.99999999999999289 ) ) ;
#13802 = PLANE ( 'NONE',  #7560 ) ;
#13803 = CARTESIAN_POINT ( 'NONE',  ( -11.73070664223723902, 301.3073905601784759, 11.32908994701042005 ) ) ;
#13804 = CARTESIAN_POINT ( 'NONE',  ( -28.68588794268869435, 193.9102039777116602, 0.000000000000000000 ) ) ;
#13805 = CARTESIAN_POINT ( 'NONE',  ( -43.68588794268869435, 210.1437886375728965, 2.161863591991830530E-19 ) ) ;
#13806 = VECTOR ( 'NONE', #20774, 1000.000000000000000 ) ;
#13807 = DIRECTION ( 'NONE',  ( 0.000000000000000000, -1.000000000000000000, 0.000000000000000000 ) ) ;
#13808 = FACE_OUTER_BOUND ( 'NONE', #2533, .T. ) ;
#13809 = DIRECTION ( 'NONE',  ( -1.191790137725560488E-16, 1.000000000000000000, -0.000000000000000000 ) ) ;
#13810 = CARTESIAN_POINT ( 'NONE',  ( -16.84014894278197971, 271.6198905683720568, -11.84573899990672707 ) ) ;
#13811 = EDGE_CURVE ( 'NONE', #13749, #13314, #17269, .T. ) ;
#13812 = CARTESIAN_POINT ( 'NONE',  ( -24.70764059509554755, 254.4323905601784759, -19.99999999999999289 ) ) ;
#13813 = CARTESIAN_POINT ( 'NONE',  ( -36.33955658999051508, 363.8698905765656377, 18.47759065022572500 ) ) ;
#13814 = CARTESIAN_POINT ( 'NONE',  ( -28.68588794268872277, 447.8698905683720000, 16.75240474999999307 ) ) ;
#13815 = DIRECTION ( 'NONE',  ( 0.000000000000000000, -0.5000000000000008882, 0.8660254037844381525 ) ) ;
#13816 = CARTESIAN_POINT ( 'NONE',  ( -42.88789093042842637, 276.3073905683720568, 9.489475012073736337 ) ) ;
#13817 = VERTEX_POINT ( 'NONE', #14382 ) ;
#13818 = CARTESIAN_POINT ( 'NONE',  ( -48.68588794268869435, 267.2448905601784759, 0.000000000000000000 ) ) ;
#13819 = CARTESIAN_POINT ( 'NONE',  ( -22.27502019258949062, 478.4948905683720000, 15.47720386886985189 ) ) ;
#13820 = VECTOR ( 'NONE', #13793, 1000.000000000000000 ) ;
#13821 = EDGE_LOOP ( 'NONE', ( #5289, #11230, #10653, #10981 ) ) ;
#13822 = DIRECTION ( 'NONE',  ( -1.000000000000000000, 0.000000000000000000, 0.000000000000000000 ) ) ;
#13823 = CARTESIAN_POINT ( 'NONE',  ( -40.53162694259542320, 262.6198905683720568, -11.84573899990672707 ) ) ;
#13824 = ORIENTED_EDGE ( 'NONE', *, *, #12784, .T. ) ;
#13825 = PLANE ( 'NONE',  #16637 ) ;
#13826 = CARTESIAN_POINT ( 'NONE',  ( -48.68588794268872277, 491.9948905765656377, 0.000000000000000000 ) ) ;
#13827 = CARTESIAN_POINT ( 'NONE',  ( -14.54375231895776466, 308.2448905765656377, -14.14213562373094746 ) ) ;
#13828 = CARTESIAN_POINT ( 'NONE',  ( -8.685887942688555796, 452.5573905601784190, -3.978247347592740013 ) ) ;
#13829 = CARTESIAN_POINT ( 'NONE',  ( -45.43829269268869808, 235.3698905683720284, 0.000000000000000000 ) ) ;
#13830 = CARTESIAN_POINT ( 'NONE',  ( -11.93348319268874036, 520.0573905683719431, 3.332260488124728415 ) ) ;
#13831 = DIRECTION ( 'NONE',  ( -0.000000000000000000, -0.000000000000000000, 1.000000000000000000 ) ) ;
#13832 = CARTESIAN_POINT ( 'NONE',  ( -11.93348319268870839, 249.1823905683720568, -3.332260488124732856 ) ) ;
#13833 = CARTESIAN_POINT ( 'NONE',  ( -45.43829269268871229, 345.3698905683720568, 0.000000000000000000 ) ) ;
#13834 = DIRECTION ( 'NONE',  ( 1.000000000000000000, 0.000000000000000000, 0.000000000000000000 ) ) ;
#13835 =( GEOMETRIC_REPRESENTATION_CONTEXT ( 3 ) GLOBAL_UNCERTAINTY_ASSIGNED_CONTEXT ( ( #1657 ) ) GLOBAL_UNIT_ASSIGNED_CONTEXT ( ( #14638, #9319, #16254 ) ) REPRESENTATION_CONTEXT ( 'NONE', 'WORKASPACE' ) );
#13836 = CIRCLE ( 'NONE', #4510, 9.999999999999994671 ) ;
#13837 = CARTESIAN_POINT ( 'NONE',  ( -45.43829269268871229, 403.5573905683720000, -3.332260488124726194 ) ) ;
#13838 = CARTESIAN_POINT ( 'NONE',  ( -10.20829729246298179, 326.3698905765656377, 7.653668647301790529 ) ) ;
#13839 = CARTESIAN_POINT ( 'NONE',  ( -45.64106924314019409, 408.1823905601784759, 11.32908994701042715 ) ) ;
#13840 = ORIENTED_EDGE ( 'NONE', *, *, #18917, .T. ) ;
#13841 = CARTESIAN_POINT ( 'NONE',  ( -21.03221929538692336, 348.8698905765656377, -18.47759065022572855 ) ) ;
#13842 = ORIENTED_EDGE ( 'NONE', *, *, #15446, .T. ) ;
#13843 = VERTEX_POINT ( 'NONE', #16101 ) ;
#13844 = CARTESIAN_POINT ( 'NONE',  ( -22.27502019258949417, 498.4948905683720568, 15.47720386886985189 ) ) ;
#13845 = CARTESIAN_POINT ( 'NONE',  ( -17.35679799567828496, 290.6823905601785327, 16.95518130045146421 ) ) ;
#13846 = CARTESIAN_POINT ( 'NONE',  ( -21.03221929538691981, 318.8698905765656377, -18.47759065022572855 ) ) ;
#13847 = VECTOR ( 'NONE', #1480, 1000.000000000000000 ) ;
#13848 = ORIENTED_EDGE ( 'NONE', *, *, #1969, .T. ) ;
#13849 = EDGE_CURVE ( 'NONE', #12831, #2272, #15115, .T. ) ;
#13850 = CARTESIAN_POINT ( 'NONE',  ( -44.16309181155856578, 324.7448905683720000, -6.410867750099231266 ) ) ;
#13851 = AXIS2_PLACEMENT_3D ( 'NONE', #11178, #9551, #17780 ) ;
#13852 = VERTEX_POINT ( 'NONE', #19441 ) ;
#13853 = CARTESIAN_POINT ( 'NONE',  ( -35.09675569278794427, 351.9948905683720000, -15.47720386886985544 ) ) ;
#13854 = EDGE_CURVE ( 'NONE', #19602, #13635, #15970, .T. ) ;
#13855 = CARTESIAN_POINT ( 'NONE',  ( -32.01814843081344719, 356.0573905683719431, 16.75240474999999307 ) ) ;
#13856 = ADVANCED_FACE ( 'NONE', ( #15128 ), #5048, .F. ) ;
#13857 = EDGE_CURVE ( 'NONE', #6220, #13843, #10017, .T. ) ;
#13858 = CARTESIAN_POINT ( 'NONE',  ( -11.73070664223724080, 287.9323905765655809, -11.32908994701042715 ) ) ;
#13859 = CIRCLE ( 'NONE', #4525, 4.400000000000000355 ) ;
#13860 = CARTESIAN_POINT ( 'NONE',  ( -21.03221929538694113, 498.8698905765656377, -18.47759065022572855 ) ) ;
#13861 = CARTESIAN_POINT ( 'NONE',  ( -35.09675569278793716, 255.7448905683720284, 15.47720386886985366 ) ) ;
#13862 = CARTESIAN_POINT ( 'NONE',  ( -47.16347859291443001, 226.6198905601785043, -7.653668647301793193 ) ) ;
#13863 = CARTESIAN_POINT ( 'NONE',  ( -28.68588794268872277, 422.8698905683720568, -16.75240474999999307 ) ) ;
#13864 = FACE_OUTER_BOUND ( 'NONE', #16129, .T. ) ;
#13865 = CARTESIAN_POINT ( 'NONE',  ( -42.82802356641967378, 450.7448905765656377, -14.14213562373094746 ) ) ;
#13866 = CARTESIAN_POINT ( 'NONE',  ( 0.000000000000000000, 0.000000000000000000, 0.000000000000000000 ) ) ;
#13867 = EDGE_CURVE ( 'NONE', #4551, #13714, #1518, .T. ) ;
#13868 = CARTESIAN_POINT ( 'NONE',  ( -13.20868407381885490, 320.9948905683720568, -6.410867750099233042 ) ) ;
#13869 = CARTESIAN_POINT ( 'NONE',  ( -40.53162694259545162, 455.1198905683720568, 11.84573899990672885 ) ) ;
#13870 = VERTEX_POINT ( 'NONE', #8502 ) ;
#13871 = CARTESIAN_POINT ( 'NONE',  ( -42.82802356641967378, 475.9948905601784759, -14.14213562373094746 ) ) ;
#13872 = CARTESIAN_POINT ( 'NONE',  ( -16.84014894278197971, 280.1198905683720000, -11.84573899990672707 ) ) ;
#13873 = VERTEX_POINT ( 'NONE', #13393 ) ;
#13874 = AXIS2_PLACEMENT_3D ( 'NONE', #3364, #16245, #13320 ) ;
#13875 = LINE ( 'NONE', #20464, #20165 ) ;
#13876 = CARTESIAN_POINT ( 'NONE',  ( -45.43829269268871940, 445.3698905683720000, 0.000000000000000000 ) ) ;
#13877 = ORIENTED_EDGE ( 'NONE', *, *, #16765, .T. ) ;
#13878 = DIRECTION ( 'NONE',  ( -0.9362971185447991340, 0.000000000000000000, -0.3512089204514979301 ) ) ;
#13879 = CARTESIAN_POINT ( 'NONE',  ( -14.48388495494899431, 309.8073905683720568, -9.489475012073736337 ) ) ;
#13880 = CARTESIAN_POINT ( 'NONE',  ( -14.48388495494900674, 391.3073905683720568, -9.489475012073734561 ) ) ;
#13881 = CARTESIAN_POINT ( 'NONE',  ( -28.68588794268875475, 600.7448905601785327, 0.000000000000000000 ) ) ;
#13882 = CARTESIAN_POINT ( 'NONE',  ( -17.35679799567830983, 515.4323905765655809, 16.95518130045146421 ) ) ;
#13883 = CARTESIAN_POINT ( 'NONE',  ( -35.09675569278795138, 401.9948905683720568, -15.47720386886985544 ) ) ;
#13884 = CARTESIAN_POINT ( 'NONE',  ( -45.43829269268869098, 235.0573905683720568, -3.332260488124726194 ) ) ;
#13885 = CARTESIAN_POINT ( 'NONE',  ( -16.84014894278199392, 427.6198905683720000, 11.84573899990672530 ) ) ;
#13886 =( BOUNDED_CURVE ( )  B_SPLINE_CURVE ( 2, ( #1534, #8104, #4875, #11469, #18067, #8216, #14844, #16043, #20, #2047, #5696, #3865, #13827, #3757, #17182, #10665, #8620 ),
 .UNSPECIFIED., .F., .T. ) 
 B_SPLINE_CURVE_WITH_KNOTS ( ( 3, 2, 2, 2, 2, 2, 2, 2, 3 ),
 ( 0.6875000000000002220, 0.6894531250000002220, 0.6914062500000002220, 0.6933593750000002220, 0.6953125000000002220, 0.6972656250000002220, 0.6992187500000002220, 0.7011718750000002220, 0.7031250000000002220 ),
 .UNSPECIFIED. ) 
 CURVE ( )  GEOMETRIC_REPRESENTATION_ITEM ( )  RATIONAL_B_SPLINE_CURVE ( ( 0.9999999999999977796, 0.9807852804032326510, 1.000000000000000000, 0.9807852804032304306, 1.000000000000000000, 0.9807852804032304306, 1.000000000000000000, 0.9807852804032304306, 1.000000000000000000, 0.9807852804032304306, 1.000000000000000000, 0.9807852804032304306, 1.000000000000000000, 0.9807852804032304306, 1.000000000000000000, 0.9807852804032282101, 1.000000000000002220 ) ) 
 REPRESENTATION_ITEM ( '' )  );
#13887 = CARTESIAN_POINT ( 'NONE',  ( -21.03221929538690915, 345.1198905765656377, 18.47759065022572500 ) ) ;
#13888 = LINE ( 'NONE', #2203, #12750 ) ;
#13889 = CARTESIAN_POINT ( 'NONE',  ( -32.01814843081344719, 336.0573905683720568, 16.75240474999999307 ) ) ;
#13890 = CARTESIAN_POINT ( 'NONE',  ( -22.27502019258949062, 478.4948905683720000, 15.47720386886985189 ) ) ;
#13891 = CARTESIAN_POINT ( 'NONE',  ( -8.685887942688740537, 516.9948905765655809, -2.449293598294705724E-15 ) ) ;
#13892 = LINE ( 'NONE', #8794, #7632 ) ;
#13893 = VECTOR ( 'NONE', #16537, 1000.000000000000000 ) ;
#13894 = FACE_OUTER_BOUND ( 'NONE', #9811, .T. ) ;
#13895 = VECTOR ( 'NONE', #6101, 1000.000000000000000 ) ;
#13896 = CARTESIAN_POINT ( 'NONE',  ( -11.93348319268872437, 390.3698905683720568, -2.051577885510841163E-15 ) ) ;
#13897 = CARTESIAN_POINT ( 'NONE',  ( -174.5421710038924346, 600.7448905601785327, -96.70028278950395872 ) ) ;
#13898 = CARTESIAN_POINT ( 'NONE',  ( -48.68588794268872988, 527.5573905601784190, 3.978247347593168115 ) ) ;
#13899 = CARTESIAN_POINT ( 'NONE',  ( -45.43829269268871229, 343.8698905683720000, 0.000000000000000000 ) ) ;
#13900 = VERTEX_POINT ( 'NONE', #8175 ) ;
#13901 = CARTESIAN_POINT ( 'NONE',  ( -28.68588794268872988, 506.3698905683720000, 16.75240474999999307 ) ) ;
#13902 = VERTEX_POINT ( 'NONE', #14806 ) ;
#13903 = CARTESIAN_POINT ( 'NONE',  ( -47.16347859291444422, 356.6198905601784759, -7.653668647301793193 ) ) ;
#13904 = CARTESIAN_POINT ( 'NONE',  ( -45.44977940338448974, 223.9102039777116602, -0.2342134211204321415 ) ) ;
#13905 = DIRECTION ( 'NONE',  ( -1.191790137725560488E-16, 1.000000000000000000, -0.000000000000000000 ) ) ;
#13906 = CARTESIAN_POINT ( 'NONE',  ( -11.73070664223724080, 287.9323905765655809, -11.32908994701042538 ) ) ;
#13907 = CARTESIAN_POINT ( 'NONE',  ( -36.33955658999052929, 520.1198905765655809, -18.47759065022572855 ) ) ;
#13908 = CARTESIAN_POINT ( 'NONE',  ( -32.01814843081346140, 471.6823905683720568, -16.75240474999999307 ) ) ;
#13909 = VECTOR ( 'NONE', #21145, 1000.000000000000114 ) ;
#13910 = ORIENTED_EDGE ( 'NONE', *, *, #6887, .F. ) ;
#13911 = CARTESIAN_POINT ( 'NONE',  ( -13.20868407381887266, 478.2448905683720568, 6.410867750099229490 ) ) ;
#13912 = CARTESIAN_POINT ( 'NONE',  ( -11.73070664223723192, 246.0573905765656093, 11.32908994701042005 ) ) ;
#13913 = EDGE_CURVE ( 'NONE', #4442, #534, #2656, .T. ) ;
#13914 = CARTESIAN_POINT ( 'NONE',  ( -24.70764059509556887, 409.1823905765655809, -19.99999999999999289 ) ) ;
#13915 = CARTESIAN_POINT ( 'NONE',  ( -43.68588794268873698, 588.2448905601785327, 1.836970198721029589E-15 ) ) ;
#13916 = LINE ( 'NONE', #5460, #11986 ) ;
#13917 = DIRECTION ( 'NONE',  ( 0.000000000000000000, -1.000000000000000000, 0.000000000000000000 ) ) ;
#13918 = CARTESIAN_POINT ( 'NONE',  ( -42.82802356641967378, 483.2448905765656377, 14.14213562373094923 ) ) ;
#13919 = CARTESIAN_POINT ( 'NONE',  ( 43.53705524234220547, 30.52886280891152282, 96.62835994548002816 ) ) ;
#13920 = CARTESIAN_POINT ( 'NONE',  ( -32.66413529028185536, 239.4323905601785043, 19.99999999999999289 ) ) ;
#13921 = EDGE_CURVE ( 'NONE', #9782, #12347, #6555, .T. ) ;
#13922 = CARTESIAN_POINT ( 'NONE',  ( 147.4234352242185935, 620.7448905601785327, 1.893624729818134345 ) ) ;
#13923 = VECTOR ( 'NONE', #11287, 999.9999999999998863 ) ;
#13924 = CARTESIAN_POINT ( 'NONE',  ( -19.19641293061497578, 281.9323905683720568, -14.20200298773971603 ) ) ;
#13925 = CARTESIAN_POINT ( 'NONE',  ( -45.64106924314017277, 246.3073905601784759, -11.32908994701042715 ) ) ;
#13926 = CARTESIAN_POINT ( 'NONE',  ( -32.66413529028186957, 364.1823905765656377, 19.99999999999999289 ) ) ;
#13927 = CARTESIAN_POINT ( 'NONE',  ( -44.16309181155858710, 454.7448905683720568, -6.410867750099231266 ) ) ;
#13928 = CARTESIAN_POINT ( 'NONE',  ( -40.01497788969914637, 400.4323905765655809, -16.95518130045146421 ) ) ;
#13929 = CARTESIAN_POINT ( 'NONE',  ( -45.43829269268869808, 275.0573905683720568, -3.332260488124726194 ) ) ;
#13930 = ORIENTED_EDGE ( 'NONE', *, *, #18591, .T. ) ;
#13931 = DIRECTION ( 'NONE',  ( 0.000000000000000000, -1.000000000000000000, 0.000000000000000000 ) ) ;
#13932 = VERTEX_POINT ( 'NONE', #3327 ) ;
#13933 = CARTESIAN_POINT ( 'NONE',  ( -38.17536295476246977, 483.8073905683720000, -14.20200298773971426 ) ) ;
#13934 = B_SPLINE_CURVE_WITH_KNOTS ( 'NONE', 3,
 ( #7463, #15609, #12348, #15713, #5849, #17326 ),
 .UNSPECIFIED., .F., .F.,
 ( 4, 2, 4 ),
 ( 0.02294124189247800580, 0.02484059228080998452, 0.02673994266914196671 ),
 .UNSPECIFIED. ) ;
#13935 = ORIENTED_EDGE ( 'NONE', *, *, #18002, .T. ) ;
#13936 = CARTESIAN_POINT ( 'NONE',  ( 4.700000000000000178, 6.500000000000000888, 0.000000000000000000 ) ) ;
#13937 = CARTESIAN_POINT ( 'NONE',  ( -19.19641293061497223, 240.4323905683720284, -14.20200298773971603 ) ) ;
#13938 = VECTOR ( 'NONE', #12236, 1000.000000000000000 ) ;
#13939 = ORIENTED_EDGE ( 'NONE', *, *, #4688, .T. ) ;
#13940 = CARTESIAN_POINT ( 'NONE',  ( -73.08746600497821078, 585.7448905601785327, -22.98912494155474207 ) ) ;
#13941 = EDGE_CURVE ( 'NONE', #16379, #11812, #16748, .T. ) ;
#13942 = CARTESIAN_POINT ( 'NONE',  ( -42.82802356641967378, 473.2448905765655809, 14.14213562373094923 ) ) ;
#13943 = CARTESIAN_POINT ( 'NONE',  ( -8.685887942688905738, 391.9323905601784759, 3.978247347593586447 ) ) ;
#13944 = CARTESIAN_POINT ( 'NONE',  ( 51.50493485826542184, 170.1716627696692683, 57.52045949366692668 ) ) ;
#13945 = LINE ( 'NONE', #9268, #17795 ) ;
#13946 = CARTESIAN_POINT ( 'NONE',  ( -42.88789093042845479, 516.3073905683720568, 9.489475012073736337 ) ) ;
#13947 = CARTESIAN_POINT ( 'NONE',  ( -36.33955658999051508, 373.8698905765656377, 18.47759065022572500 ) ) ;
#13948 = CARTESIAN_POINT ( 'NONE',  ( -44.16309181155855157, 254.4948905683720568, 6.410867750099241924 ) ) ;
#13949 = CARTESIAN_POINT ( 'NONE',  ( -22.27502019258948351, 332.2448905683720568, -15.47720386886985544 ) ) ;
#13950 = AXIS2_PLACEMENT_3D ( 'NONE', #20760, #1287, #14492 ) ;
#13951 = PLANE ( 'NONE',  #6786 ) ;
#13952 = CARTESIAN_POINT ( 'NONE',  ( -48.68588794268887199, 302.3073905765655240, 3.978247347592742678 ) ) ;
#13953 = AXIS2_PLACEMENT_3D ( 'NONE', #11286, #3297, #12924 ) ;
#13954 = EDGE_CURVE ( 'NONE', #10309, #21365, #18457, .T. ) ;
#13955 = CARTESIAN_POINT ( 'NONE',  ( -32.01814843081345430, 401.6823905683720000, -16.75240474999999307 ) ) ;
#13956 = UNCERTAINTY_MEASURE_WITH_UNIT (LENGTH_MEASURE( 1.000000000000000082E-05 ), #16948, 'distance_accuracy_value', 'NONE');
#13957 = LINE ( 'NONE', #3876, #10479 ) ;
#13958 = CARTESIAN_POINT ( 'NONE',  ( -17.35679799567830273, 383.8073905601784190, -16.95518130045146421 ) ) ;
#13959 = ORIENTED_EDGE ( 'NONE', *, *, #15256, .F. ) ;
#13960 = CARTESIAN_POINT ( 'NONE',  ( -32.66413529028186957, 349.8073905765655809, -19.99999999999999289 ) ) ;
#13961 = VERTEX_POINT ( 'NONE', #10228 ) ;
#13962 = ORIENTED_EDGE ( 'NONE', *, *, #13954, .F. ) ;
#13963 = CARTESIAN_POINT ( 'NONE',  ( -42.88789093042845479, 516.3073905683720568, 9.489475012073736337 ) ) ;
#13964 = CARTESIAN_POINT ( 'NONE',  ( -8.685887942688724550, 382.2448905601784759, -2.449293598294705724E-15 ) ) ;
#13965 = ORIENTED_EDGE ( 'NONE', *, *, #6044, .T. ) ;
#13966 = EDGE_CURVE ( 'NONE', #6673, #9723, #18154, .T. ) ;
#13967 = AXIS2_PLACEMENT_3D ( 'NONE', #17354, #928, #1138 ) ;
#13968 = CARTESIAN_POINT ( 'NONE',  ( -25.35362745456398414, 302.5573905683720568, -16.75240474999999307 ) ) ;
#13969 = VERTEX_POINT ( 'NONE', #2036 ) ;
#13970 = CARTESIAN_POINT ( 'NONE',  ( -16.84014894278198682, 340.1198905683720568, -11.84573899990672707 ) ) ;
#13971 = CARTESIAN_POINT ( 'NONE',  ( -19.19641293061497933, 347.3073905683720568, 14.20200298773971426 ) ) ;
#13972 = AXIS2_PLACEMENT_3D ( 'NONE', #9278, #15895, #10677 ) ;
#13973 = CARTESIAN_POINT ( 'NONE',  ( -8.685887942688712116, 276.9948905765656377, -2.449293598294705724E-15 ) ) ;
#13974 = CARTESIAN_POINT ( 'NONE',  ( -14.54375231895778775, 498.2448905765656377, -14.14213562373094746 ) ) ;
#13975 = CARTESIAN_POINT ( 'NONE',  ( -32.01814843081343298, 241.6823905683720568, -16.75240474999999307 ) ) ;
#13976 = CARTESIAN_POINT ( 'NONE',  ( -43.04679578547633412, 202.6324317550694332, 4.335932898175371086 ) ) ;
#13977 = CARTESIAN_POINT ( 'NONE',  ( -11.93348319268872615, 400.6823905683720568, -3.332260488124732856 ) ) ;
#13978 = CARTESIAN_POINT ( 'NONE',  ( 21.30000000000000071, 0.000000000000000000, 0.000000000000000000 ) ) ;
#13979 = CARTESIAN_POINT ( 'NONE',  ( -32.66413529028188378, 449.8073905765656377, -19.99999999999999289 ) ) ;
#13980 = CARTESIAN_POINT ( 'NONE',  ( -44.16309181155858710, 453.2448905683720000, -6.410867750099231266 ) ) ;
#13981 = ORIENTED_EDGE ( 'NONE', *, *, #10224, .T. ) ;
#13982 = CARTESIAN_POINT ( 'NONE',  ( -8.685887942688731655, 452.2448905601784759, -2.449293598294705724E-15 ) ) ;
#13983 = CARTESIAN_POINT ( 'NONE',  ( -11.93348319268871371, 279.1823905683720000, -3.332260488124732856 ) ) ;
#13984 = AXIS2_PLACEMENT_3D ( 'NONE', #20039, #11815, #5316 ) ;
#13985 = ORIENTED_EDGE ( 'NONE', *, *, #16976, .F. ) ;
#13986 = CARTESIAN_POINT ( 'NONE',  ( -21.03221929538690560, 340.3698905601784759, 18.47759065022572500 ) ) ;
#13987 = ORIENTED_EDGE ( 'NONE', *, *, #8517, .F. ) ;
#13988 = ORIENTED_EDGE ( 'NONE', *, *, #9568, .T. ) ;
#13989 = CARTESIAN_POINT ( 'NONE',  ( -28.68588794268874054, 573.2448905601785327, 0.000000000000000000 ) ) ;
#13990 = CARTESIAN_POINT ( 'NONE',  ( -13.20868407381885312, 299.4948905683720568, -6.410867750099233042 ) ) ;
#13991 = CARTESIAN_POINT ( 'NONE',  ( -40.53162694259543741, 364.1198905683720000, -11.84573899990672707 ) ) ;
#13992 = CARTESIAN_POINT ( 'NONE',  ( -24.70764059509555821, 374.4323905601784759, -19.99999999999999289 ) ) ;
#13993 = CARTESIAN_POINT ( 'NONE',  ( -32.66413529028189799, 514.1823905765656946, 19.99999999999999289 ) ) ;
#13994 = CARTESIAN_POINT ( 'NONE',  ( -28.68588794268872277, 411.3698905683720568, -16.75240474999999307 ) ) ;
#13995 = CARTESIAN_POINT ( 'NONE',  ( -28.68588794268870146, 232.8698905683720284, -16.75240474999999307 ) ) ;
#13996 = EDGE_CURVE ( 'NONE', #15047, #9674, #9035, .T. ) ;
#13997 = CARTESIAN_POINT ( 'NONE',  ( -32.01814843081344719, 416.0573905683721136, 16.75240474999999307 ) ) ;
#13998 = EDGE_CURVE ( 'NONE', #11378, #12297, #3264, .T. ) ;
#13999 = CARTESIAN_POINT ( 'NONE',  ( -48.68588794268870856, 351.6823905765656377, -3.978247347593158345 ) ) ;
#14000 = DIRECTION ( 'NONE',  ( -0.4627175328665442677, 0.000000000000000000, 0.8865057725575725689 ) ) ;
#14001 = CARTESIAN_POINT ( 'NONE',  ( -25.35362745456398414, 311.0573905683720568, -16.75240474999999307 ) ) ;
#14002 =( NAMED_UNIT ( * ) PLANE_ANGLE_UNIT ( ) SI_UNIT ( $, .RADIAN. ) );
#14003 = CARTESIAN_POINT ( 'NONE',  ( -22.27502019258949773, 462.2448905683720568, -15.47720386886985544 ) ) ;
#14004 = CARTESIAN_POINT ( 'NONE',  ( -36.33955658999053639, 513.8698905765655809, 18.47759065022572500 ) ) ;
#14005 = DIRECTION ( 'NONE',  ( -0.3717199501173604759, 0.000000000000000000, -0.9283449136418786551 ) ) ;
#14006 = CARTESIAN_POINT ( 'NONE',  ( 0.000000000000000000, 10.52886280891152104, 0.000000000000000000 ) ) ;
#14007 = CARTESIAN_POINT ( 'NONE',  ( -44.16309181155857289, 364.7448905683720568, -6.410867750099231266 ) ) ;
#14008 = CARTESIAN_POINT ( 'NONE',  ( 5.700000000000000178, 5.388445916248354013E-16, 4.400000000000000355 ) ) ;
#14009 = CARTESIAN_POINT ( 'NONE',  ( -8.685887942688744090, 531.9323905601785327, 3.978247347593161010 ) ) ;
#14010 = CARTESIAN_POINT ( 'NONE',  ( -11.93348319268871904, 348.8698905683720568, -2.051577885510841163E-15 ) ) ;
#14011 = ORIENTED_EDGE ( 'NONE', *, *, #6887, .T. ) ;
#14012 = CARTESIAN_POINT ( 'NONE',  ( -11.93348319268873858, 498.5573905683720568, 3.332260488124728415 ) ) ;
#14013 = ORIENTED_EDGE ( 'NONE', *, *, #7586, .T. ) ;
#14014 =( BOUNDED_CURVE ( )  B_SPLINE_CURVE ( 2, ( #19866, #5043, #3639, #10221, #16846, #7081, #3847, #5893, #20295, #20399, #8921, #18765, #3953, #17056, #17370, #7403, #14029 ),
 .UNSPECIFIED., .F., .T. ) 
 B_SPLINE_CURVE_WITH_KNOTS ( ( 3, 2, 2, 2, 2, 2, 2, 2, 3 ),
 ( 0.3125000000000001110, 0.3144531250000001110, 0.3164062500000001110, 0.3183593750000001110, 0.3203125000000001110, 0.3222656250000001110, 0.3242187500000001110, 0.3261718750000001110, 0.3281250000000001110 ),
 .UNSPECIFIED. ) 
 CURVE ( )  GEOMETRIC_REPRESENTATION_ITEM ( )  RATIONAL_B_SPLINE_CURVE ( ( 0.9999999999999988898, 0.9807852804032315408, 1.000000000000000000, 0.9807852804032304306, 1.000000000000000000, 0.9807852804032304306, 1.000000000000000000, 0.9807852804032304306, 1.000000000000000000, 0.9807852804032304306, 1.000000000000000000, 0.9807852804032304306, 1.000000000000000000, 0.9807852804032304306, 1.000000000000000000, 0.9807852804032293204, 1.000000000000001110 ) ) 
 REPRESENTATION_ITEM ( '' )  );
#14015 = CARTESIAN_POINT ( 'NONE',  ( -40.01497788969913927, 380.4323905765655240, -16.95518130045146421 ) ) ;
#14016 = CARTESIAN_POINT ( 'NONE',  ( -14.54375231895776110, 315.7448905765656377, 14.14213562373094568 ) ) ;
#14017 = LINE ( 'NONE', #18968, #17631 ) ;
#14018 = CARTESIAN_POINT ( 'NONE',  ( 0.000000000000000000, 10.52886280891152104, 0.000000000000000000 ) ) ;
#14019 = CARTESIAN_POINT ( 'NONE',  ( -11.93348319268873503, 468.8698905683720000, -2.051577885510841163E-15 ) ) ;
#14020 = ORIENTED_EDGE ( 'NONE', *, *, #10803, .F. ) ;
#14021 = CARTESIAN_POINT ( 'NONE',  ( -32.01814843081345430, 466.0573905683720568, 16.75240474999999307 ) ) ;
#14022 = CARTESIAN_POINT ( 'NONE',  ( 0.4033376246892473316, 4.059728990630800283, 5.968343123267133343 ) ) ;
#14023 = CARTESIAN_POINT ( 'NONE',  ( -10.20829729246299067, 406.3698905765656377, 7.653668647301790529 ) ) ;
#14024 = LINE ( 'NONE', #7504, #5834 ) ;
#14025 = CARTESIAN_POINT ( 'NONE',  ( -28.68588794268874054, 333.8848358243226357, -40.00000000000000000 ) ) ;
#14026 = CARTESIAN_POINT ( 'NONE',  ( 0.4037800551813700012, 4.058962678540093627, -5.969670414742686226 ) ) ;
#14027 = CARTESIAN_POINT ( 'NONE',  ( -28.68588794268874054, 585.7448905601785327, 0.000000000000000000 ) ) ;
#14028 = CARTESIAN_POINT ( 'NONE',  ( -10.20829729246297468, 257.6198905765656377, -7.653668647301794969 ) ) ;
#14029 = CARTESIAN_POINT ( 'NONE',  ( -8.685887942688729879, 432.2448905601785327, -2.449293598294705724E-15 ) ) ;
#14030 = CARTESIAN_POINT ( 'NONE',  ( 88.28695088269886071, 142.5259582928263455, -20.00000000000000355 ) ) ;
#14031 = CARTESIAN_POINT ( 'NONE',  ( -45.43829269268870519, 275.3698905683720000, 0.000000000000000000 ) ) ;
#14032 = CARTESIAN_POINT ( 'NONE',  ( -24.70764059509553334, 250.0573905601785043, 19.99999999999998934 ) ) ;
#14033 = CYLINDRICAL_SURFACE ( 'NONE', #8515, 38.00000000000000000 ) ;
#14034 = CARTESIAN_POINT ( 'NONE',  ( -8.685887942688719221, 326.9948905765656377, -2.449293598294705724E-15 ) ) ;
#14035 = CARTESIAN_POINT ( 'NONE',  ( -35.09675569278794427, 277.2448905683720568, 15.47720386886985366 ) ) ;
#14036 = ORIENTED_EDGE ( 'NONE', *, *, #5844, .T. ) ;
#14037 = CARTESIAN_POINT ( 'NONE',  ( -17.35679799567830983, 478.5573905765656377, -16.95518130045146421 ) ) ;
#14038 = ORIENTED_EDGE ( 'NONE', *, *, #14041, .T. ) ;
#14039 = CARTESIAN_POINT ( 'NONE',  ( -44.16309181155857999, 475.9948905683720000, 6.410867750099241924 ) ) ;
#14040 = ORIENTED_EDGE ( 'NONE', *, *, #2820, .T. ) ;
#14041 = EDGE_CURVE ( 'NONE', #4259, #364, #4287, .T. ) ;
#14042 = CARTESIAN_POINT ( 'NONE',  ( -10.20829729246300666, 526.3698905765656946, 7.653668647301790529 ) ) ;
#14043 = CARTESIAN_POINT ( 'NONE',  ( -11.93348319268870661, 238.8698905683720568, -2.051577885510841163E-15 ) ) ;
#14044 = EDGE_LOOP ( 'NONE', ( #4678, #17842, #20492, #12324 ) ) ;
#14045 = LINE ( 'NONE', #747, #14547 ) ;
#14046 = CARTESIAN_POINT ( 'NONE',  ( -42.82802356641967378, 463.2448905765656377, 14.14213562373094923 ) ) ;
#14047 = DIRECTION ( 'NONE',  ( 0.000000000000000000, 1.000000000000000000, 0.000000000000000000 ) ) ;
#14048 = CARTESIAN_POINT ( 'NONE',  ( 6.416697501590670427, 217.7548513357008630, -60.00000000000000000 ) ) ;
#14049 = CARTESIAN_POINT ( 'NONE',  ( -20.38821492105416056, 223.9102039777116602, -17.94255365484195508 ) ) ;
#14050 = CARTESIAN_POINT ( 'NONE',  ( -45.43829269268869808, 225.6823905683720284, 3.332260488124734632 ) ) ;
#14051 = CARTESIAN_POINT ( 'NONE',  ( -45.43829269268873361, 525.3698905683720568, 0.000000000000000000 ) ) ;
#14052 = CARTESIAN_POINT ( 'NONE',  ( -48.68588794268887199, 372.3073905765655809, 3.978247347592742678 ) ) ;
#14053 = CARTESIAN_POINT ( 'NONE',  ( -44.16309181155855157, 244.4948905683720284, 6.410867750099241924 ) ) ;
#14054 = CARTESIAN_POINT ( 'NONE',  ( -19.19641293061497933, 338.8073905683720000, 14.20200298773971426 ) ) ;
#14055 = DIRECTION ( 'NONE',  ( 0.000000000000000000, 1.000000000000000000, 0.000000000000000000 ) ) ;
#14056 = CARTESIAN_POINT ( 'NONE',  ( -8.685887942688887975, 276.6823905765655809, 3.978247347593586447 ) ) ;
#14057 = EDGE_CURVE ( 'NONE', #6373, #3963, #10441, .T. ) ;
#14058 = VECTOR ( 'NONE', #5867, 1000.000000000000114 ) ;
#14059 = CARTESIAN_POINT ( 'NONE',  ( -11.93348319268872437, 389.1823905683721136, -3.332260488124732856 ) ) ;
#14060 = CARTESIAN_POINT ( 'NONE',  ( 5.674999999999999822, -7.505553499465148271, 0.000000000000000000 ) ) ;
#14061 = CARTESIAN_POINT ( 'NONE',  ( -32.66413529028187668, 385.0573905601784190, -19.99999999999999289 ) ) ;
#14062 = ORIENTED_EDGE ( 'NONE', *, *, #6785, .T. ) ;
#14063 = FACE_BOUND ( 'NONE', #19160, .T. ) ;
#14064 = ORIENTED_EDGE ( 'NONE', *, *, #16052, .F. ) ;
#14065 = ORIENTED_EDGE ( 'NONE', *, *, #17363, .T. ) ;
#14066 = CARTESIAN_POINT ( 'NONE',  ( -35.09675569278796559, 513.4948905683720568, -15.47720386886985544 ) ) ;
#14067 = CARTESIAN_POINT ( 'NONE',  ( 30.42502041961814996, 170.1716627696692683, -20.00000000000000355 ) ) ;
#14068 = ORIENTED_EDGE ( 'NONE', *, *, #4472, .T. ) ;
#14069 = CARTESIAN_POINT ( 'NONE',  ( -25.35362745456398414, 312.5573905683720000, -16.75240474999999307 ) ) ;
#14070 = EDGE_LOOP ( 'NONE', ( #19791, #933, #530, #17300, #8912, #4860 ) ) ;
#14071 = CARTESIAN_POINT ( 'NONE',  ( -35.09675569278795138, 335.7448905683720568, 15.47720386886985366 ) ) ;
#14072 = CARTESIAN_POINT ( 'NONE',  ( -28.68588794268871212, 341.3698905683720000, -16.75240474999999307 ) ) ;
#14073 = EDGE_CURVE ( 'NONE', #10903, #12168, #2135, .T. ) ;
#14074 = CIRCLE ( 'NONE', #19929, 38.00000000000000000 ) ;
#14075 = CARTESIAN_POINT ( 'NONE',  ( -14.54375231895775755, 285.7448905765655809, 14.14213562373094568 ) ) ;
#14076 = CARTESIAN_POINT ( 'NONE',  ( -40.01497788969914637, 395.6823905601784190, -16.95518130045146421 ) ) ;
#14077 = CARTESIAN_POINT ( 'NONE',  ( -16.84014894278197261, 237.6198905683720284, 11.84573899990672530 ) ) ;
#14078 = DIRECTION ( 'NONE',  ( 0.000000000000000000, 1.000000000000000000, -0.000000000000000000 ) ) ;
#14079 = CARTESIAN_POINT ( 'NONE',  ( -16.84014894278199037, 399.1198905683720000, 11.84573899990672530 ) ) ;
#14080 = VECTOR ( 'NONE', #17340, 1000.000000000000114 ) ;
#14081 = DIRECTION ( 'NONE',  ( 0.000000000000000000, 0.000000000000000000, 1.000000000000000000 ) ) ;
#14082 = CYLINDRICAL_SURFACE ( 'NONE', #6243, 50.00000000000000000 ) ;
#14083 = CARTESIAN_POINT ( 'NONE',  ( 30.42502041961813575, 271.1055109169419097, 20.00000000000000355 ) ) ;
#14084 = EDGE_CURVE ( 'NONE', #12627, #3036, #20300, .T. ) ;
#14085 = CARTESIAN_POINT ( 'NONE',  ( -44.16309181155857999, 433.2448905683720000, -6.410867750099231266 ) ) ;
#14086 = ORIENTED_EDGE ( 'NONE', *, *, #6959, .T. ) ;
#14087 = CARTESIAN_POINT ( 'NONE',  ( -36.33955658999052218, 439.1198905601784759, 18.47759065022572500 ) ) ;
#14088 = AXIS2_PLACEMENT_3D ( 'NONE', #18650, #15331, #10321 ) ;
#14089 = VERTEX_POINT ( 'NONE', #8716 ) ;
#14090 = DIRECTION ( 'NONE',  ( -1.191790137725560488E-16, 1.000000000000000000, -0.000000000000000000 ) ) ;
#14091 = ORIENTED_EDGE ( 'NONE', *, *, #199, .T. ) ;
#14092 = EDGE_LOOP ( 'NONE', ( #9496, #3338, #79, #19143 ) ) ;
#14093 = DIRECTION ( 'NONE',  ( -9.855701800883827197E-17, 1.000000000000000000, 9.855701800883827197E-17 ) ) ;
#14094 = CARTESIAN_POINT ( 'NONE',  ( -47.16347859291443712, 317.8698905601784190, 7.653668647301805628 ) ) ;
#14095 = CARTESIAN_POINT ( 'NONE',  ( -19.19641293061497578, 297.3073905683720568, 14.20200298773971426 ) ) ;
#14096 = VECTOR ( 'NONE', #3477, 1000.000000000000000 ) ;
#14097 = CARTESIAN_POINT ( 'NONE',  ( -45.43829269268871229, 355.6823905683720568, 3.332260488124734632 ) ) ;
#14098 = CARTESIAN_POINT ( 'NONE',  ( 125.7989814974898337, 160.1716627696691830, -40.00000000000000000 ) ) ;
#14099 = CARTESIAN_POINT ( 'NONE',  ( -32.66413529028189799, 529.8073905765656946, -19.99999999999999289 ) ) ;
#14100 = CARTESIAN_POINT ( 'NONE',  ( -42.88789093042844058, 404.8073905683721136, 9.489475012073736337 ) ) ;
#14101 = CARTESIAN_POINT ( 'NONE',  ( -45.43829269268869808, 245.3698905683720568, 0.000000000000000000 ) ) ;
#14102 = CARTESIAN_POINT ( 'NONE',  ( -11.93348319268872615, 408.5573905683721136, 3.332260488124728859 ) ) ;
#14103 = CARTESIAN_POINT ( 'NONE',  ( -40.01497788969913216, 343.5573905765655809, 16.95518130045146776 ) ) ;
#14104 = CARTESIAN_POINT ( 'NONE',  ( -21.03221929538691981, 324.1198905601784759, -18.47759065022572855 ) ) ;
#14105 = CARTESIAN_POINT ( 'NONE',  ( -28.68588794268870501, 296.3698905683720568, 16.75240474999999307 ) ) ;
#14106 = CARTESIAN_POINT ( 'NONE',  ( -45.43829269268872650, 465.3698905683720000, 0.000000000000000000 ) ) ;
#14107 = CARTESIAN_POINT ( 'NONE',  ( -14.54375231895777887, 460.9948905601785327, 14.14213562373094568 ) ) ;
#14108 = CARTESIAN_POINT ( 'NONE',  ( -42.99843930773591438, 202.9216059526226559, -4.490902998358449416 ) ) ;
#14109 = CARTESIAN_POINT ( 'NONE',  ( 0.000000000000000000, 160.1716627696692683, 0.000000000000000000 ) ) ;
#14110 = CARTESIAN_POINT ( 'NONE',  ( -38.17536295476245556, 373.8073905683720000, -14.20200298773971426 ) ) ;
#14111 = CARTESIAN_POINT ( 'NONE',  ( -22.27502019258949417, 506.9948905683721136, 15.47720386886985189 ) ) ;
#14112 = CARTESIAN_POINT ( 'NONE',  ( -28.68588794268872988, 509.7448905601784759, 19.99999999999999289 ) ) ;
#14113 = CARTESIAN_POINT ( 'NONE',  ( -11.93348319268871904, 338.8698905683720000, -2.051577885510841163E-15 ) ) ;
#14114 = ORIENTED_EDGE ( 'NONE', *, *, #13548, .T. ) ;
#14115 = CARTESIAN_POINT ( 'NONE',  ( -28.68588794268872988, 496.3698905683720568, 16.75240474999999307 ) ) ;
#14116 = EDGE_LOOP ( 'NONE', ( #1314, #4863, #20115 ) ) ;
#14117 = CARTESIAN_POINT ( 'NONE',  ( -45.43829269268873361, 535.3698905683720568, 0.000000000000000000 ) ) ;
#14118 = CARTESIAN_POINT ( 'NONE',  ( -42.88789093042844058, 414.4323905683720000, -9.489475012073734561 ) ) ;
#14119 = CARTESIAN_POINT ( 'NONE',  ( -32.66413529028186247, 289.8073905765656946, -19.99999999999999289 ) ) ;
#14120 = CARTESIAN_POINT ( 'NONE',  ( -48.68588794268871567, 521.6823905765656946, -3.978247347593212080 ) ) ;
#14121 = CARTESIAN_POINT ( 'NONE',  ( -16.84014894278200103, 460.1198905683720568, -11.84573899990672707 ) ) ;
#14122 = ORIENTED_EDGE ( 'NONE', *, *, #18558, .F. ) ;
#14123 = CARTESIAN_POINT ( 'NONE',  ( -11.93348319268873503, 469.1823905683719431, -3.332260488124732856 ) ) ;
#14124 = CARTESIAN_POINT ( 'NONE',  ( -47.16347859291443001, 242.6198905765656377, 7.653668647301805628 ) ) ;
#14125 = ADVANCED_FACE ( 'NONE', ( #20616 ), #8823, .F. ) ;
#14126 = CARTESIAN_POINT ( 'NONE',  ( -47.16347859291445133, 401.3698905765656377, -7.653668647301793193 ) ) ;
#14127 = CARTESIAN_POINT ( 'NONE',  ( -24.70764059509554755, 279.1823905765656377, -19.99999999999999289 ) ) ;
#14128 = CARTESIAN_POINT ( 'NONE',  ( 20.42502041961806825, 281.1055109169419666, -20.00000000000000355 ) ) ;
#14129 = CARTESIAN_POINT ( 'NONE',  ( -48.68588794268872277, 467.2448905601784759, 0.000000000000000000 ) ) ;
#14130 = CARTESIAN_POINT ( 'NONE',  ( 5.299999999999999822, -3.752776749732563033, 6.500000000000000000 ) ) ;
#14131 = ADVANCED_FACE ( 'NONE', ( #18660 ), #19103, .T. ) ;
#14132 = EDGE_CURVE ( 'NONE', #126, #2082, #4766, .T. ) ;
#14133 = LINE ( 'NONE', #10968, #2660 ) ;
#14134 = CARTESIAN_POINT ( 'NONE',  ( -45.64106924314017988, 346.3073905601784759, -11.32908994701042538 ) ) ;
#14135 = CARTESIAN_POINT ( 'NONE',  ( -35.09675569278793716, 273.4948905683720000, -15.47720386886985544 ) ) ;
#14136 = AXIS2_PLACEMENT_3D ( 'NONE', #19483, #12783, #16249 ) ;
#14137 = CARTESIAN_POINT ( 'NONE',  ( -21.03221929538690915, 244.1198905601784759, -18.47759065022572855 ) ) ;
#14138 = CARTESIAN_POINT ( 'NONE',  ( 158.8141120573112630, 620.7448905601785327, 0.000000000000000000 ) ) ;
#14139 = CARTESIAN_POINT ( 'NONE',  ( -40.53162694259544452, 436.6198905683720000, 11.84573899990672885 ) ) ;
#14140 = CARTESIAN_POINT ( 'NONE',  ( -8.685887942688726326, 396.9948905765656377, -2.449293598294705724E-15 ) ) ;
#14141 = CARTESIAN_POINT ( 'NONE',  ( -45.43829269268869098, 245.0573905683720000, -3.332260488124726194 ) ) ;
#14142 = EDGE_CURVE ( 'NONE', #13421, #2991, #2454, .T. ) ;
#14143 = ORIENTED_EDGE ( 'NONE', *, *, #15503, .T. ) ;
#14144 = CARTESIAN_POINT ( 'NONE',  ( 51.50493485826542184, 170.1716627696692683, -20.00000000000000355 ) ) ;
#14145 = VERTEX_POINT ( 'NONE', #14250 ) ;
#14146 = CARTESIAN_POINT ( 'NONE',  ( -16.84014894278200458, 481.6198905683720000, -11.84573899990672707 ) ) ;
#14147 = EDGE_LOOP ( 'NONE', ( #342, #19900, #12756, #3794 ) ) ;
#14148 = CARTESIAN_POINT ( 'NONE',  ( -24.70764059509555821, 364.4323905601784759, -19.99999999999999289 ) ) ;
#14149 = CARTESIAN_POINT ( 'NONE',  ( -11.93348319268870839, 238.5573905683720000, 3.332260488124728415 ) ) ;
#14150 = VERTEX_POINT ( 'NONE', #14460 ) ;
#14151 = CARTESIAN_POINT ( 'NONE',  ( -32.01814843081346140, 521.6823905683719431, -16.75240474999999307 ) ) ;
#14152 = DIRECTION ( 'NONE',  ( 0.000000000000000000, 0.000000000000000000, -1.000000000000000000 ) ) ;
#14153 = AXIS2_PLACEMENT_3D ( 'NONE', #6310, #13247, #9868 ) ;
#14154 = CARTESIAN_POINT ( 'NONE',  ( -48.68588794268872277, 462.3073905765655809, 3.978247347593168115 ) ) ;
#14155 = DIRECTION ( 'NONE',  ( 0.000000000000000000, -0.000000000000000000, 1.000000000000000000 ) ) ;
#14156 = PRESENTATION_STYLE_ASSIGNMENT (( #4190 ) ) ;
#14157 = CARTESIAN_POINT ( 'NONE',  ( -30.27473451612855015, 223.9102039777116318, -18.25316008977560855 ) ) ;
#14158 = CARTESIAN_POINT ( 'NONE',  ( 91.21585410611801592, 31.85652257517428865, 85.46735025547120301 ) ) ;
#14159 = CARTESIAN_POINT ( 'NONE',  ( -25.35362745456399836, 508.1823905683720568, 16.75240474999998952 ) ) ;
#14160 = CARTESIAN_POINT ( 'NONE',  ( -8.685887942688902186, 376.6823905765656377, 3.978247347593586447 ) ) ;
#14161 = AXIS2_PLACEMENT_3D ( 'NONE', #12947, #6433, #9478 ) ;
#14162 = CARTESIAN_POINT ( 'NONE',  ( -35.09675569278793716, 255.7448905683720284, 15.47720386886985366 ) ) ;
#14163 = CARTESIAN_POINT ( 'NONE',  ( -42.88789093042843348, 346.3073905683720568, 9.489475012073736337 ) ) ;
#14164 = DIRECTION ( 'NONE',  ( 0.000000000000000000, 0.000000000000000000, -1.000000000000000000 ) ) ;
#14165 = CARTESIAN_POINT ( 'NONE',  ( 78.68120802659203150, 149.7457237375499517, -40.00000000000000000 ) ) ;
#14166 = AXIS2_PLACEMENT_3D ( 'NONE', #14951, #138, #19911 ) ;
#14167 = CARTESIAN_POINT ( 'NONE',  ( -45.43829269268871229, 383.8698905683720000, 0.000000000000000000 ) ) ;
#14168 = CARTESIAN_POINT ( 'NONE',  ( -17.35679799567828496, 325.4323905765656377, 16.95518130045146421 ) ) ;
#14169 = CARTESIAN_POINT ( 'NONE',  ( -8.685887942688724550, 392.5573905601785896, -3.978247347593165895 ) ) ;
#14170 = ORIENTED_EDGE ( 'NONE', *, *, #9485, .F. ) ;
#14171 = DIRECTION ( 'NONE',  ( 0.9283449136418786551, 0.000000000000000000, 0.3717199501173604759 ) ) ;
#14172 = ORIENTED_EDGE ( 'NONE', *, *, #8688, .F. ) ;
#14173 = ORIENTED_EDGE ( 'NONE', *, *, #9452, .T. ) ;
#14174 = CARTESIAN_POINT ( 'NONE',  ( -28.68588794268872988, 497.8698905683720568, 16.75240474999999307 ) ) ;
#14175 = CARTESIAN_POINT ( 'NONE',  ( -45.64106924314017277, 292.9323905765656377, 11.32908994701042538 ) ) ;
#14176 = ORIENTED_EDGE ( 'NONE', *, *, #9237, .F. ) ;
#14177 = CARTESIAN_POINT ( 'NONE',  ( -11.93348319268871549, 310.0573905683720568, 3.332260488124728859 ) ) ;
#14178 = ORIENTED_EDGE ( 'NONE', *, *, #4778, .T. ) ;
#14179 = CARTESIAN_POINT ( 'NONE',  ( -44.16309181155855867, 324.4948905683720568, 6.410867750099241924 ) ) ;
#14180 = CARTESIAN_POINT ( 'NONE',  ( -44.16309181155857289, 353.2448905683720000, -6.410867750099231266 ) ) ;
#14181 = EDGE_CURVE ( 'NONE', #15214, #2614, #14563, .T. ) ;
#14182 = CARTESIAN_POINT ( 'NONE',  ( -11.73070664223723725, 286.0573905765656377, 11.32908994701042005 ) ) ;
#14183 = LINE ( 'NONE', #8969, #15201 ) ;
#14184 = CARTESIAN_POINT ( 'NONE',  ( -38.17536295476244135, 242.3073905683720284, -14.20200298773971426 ) ) ;
#14185 = FACE_OUTER_BOUND ( 'NONE', #8658, .T. ) ;
#14186 = CARTESIAN_POINT ( 'NONE',  ( -19.19641293061498644, 398.8073905683720568, 14.20200298773971426 ) ) ;
#14187 = CARTESIAN_POINT ( 'NONE',  ( -32.66413529028186957, 335.0573905601785327, -19.99999999999999289 ) ) ;
#14188 = DIRECTION ( 'NONE',  ( 0.000000000000000000, -1.000000000000000000, 0.000000000000000000 ) ) ;
#14189 = ADVANCED_FACE ( 'NONE', ( #12616 ), #8042, .T. ) ;
#14190 = DIRECTION ( 'NONE',  ( -1.191790137725560488E-16, 1.000000000000000000, -0.000000000000000000 ) ) ;
#14191 = CARTESIAN_POINT ( 'NONE',  ( -28.68588794268872633, 451.3698905683720000, -16.75240474999999307 ) ) ;
#14192 = ORIENTED_EDGE ( 'NONE', *, *, #14654, .F. ) ;
#14193 = CARTESIAN_POINT ( 'NONE',  ( -24.70764059509556176, 450.0573905601785327, 19.99999999999998934 ) ) ;
#14194 = VERTEX_POINT ( 'NONE', #17792 ) ;
#14195 =( GEOMETRIC_REPRESENTATION_CONTEXT ( 3 ) GLOBAL_UNCERTAINTY_ASSIGNED_CONTEXT ( ( #8975 ) ) GLOBAL_UNIT_ASSIGNED_CONTEXT ( ( #15936, #5969, #19488 ) ) REPRESENTATION_CONTEXT ( 'NONE', 'WORKASPACE' ) );
#14196 = CARTESIAN_POINT ( 'NONE',  ( -8.685887942688742314, 573.2448905601785327, 2.449293598294706119E-15 ) ) ;
#14197 = VERTEX_POINT ( 'NONE', #19520 ) ;
#14198 = EDGE_CURVE ( 'NONE', #15181, #11055, #12358, .T. ) ;
#14199 = VERTEX_POINT ( 'NONE', #13035 ) ;
#14200 = DIRECTION ( 'NONE',  ( 0.4627175328665443232, 0.000000000000000000, 0.8865057725575725689 ) ) ;
#14201 = CARTESIAN_POINT ( 'NONE',  ( -17.35679799567829562, 333.8073905601784759, -16.95518130045146421 ) ) ;
#14202 = CARTESIAN_POINT ( 'NONE',  ( -16.84014894278198682, 369.1198905683720000, 11.84573899990672530 ) ) ;
#14203 = DIRECTION ( 'NONE',  ( 0.000000000000000000, 0.000000000000000000, -1.000000000000000000 ) ) ;
#14204 = VECTOR ( 'NONE', #998, 1000.000000000000000 ) ;
#14205 = CARTESIAN_POINT ( 'NONE',  ( -8.685887942688742314, 516.6823905765655809, 3.978247347593161010 ) ) ;
#14206 = CARTESIAN_POINT ( 'NONE',  ( -14.48388495494900496, 397.9323905683719431, 9.489475012073732785 ) ) ;
#14207 = CARTESIAN_POINT ( 'NONE',  ( -19.19641293061497223, 241.9323905683720284, -14.20200298773971603 ) ) ;
#14208 = AXIS2_PLACEMENT_3D ( 'NONE', #18515, #3701, #19830 ) ;
#14209 = CARTESIAN_POINT ( 'NONE',  ( -22.27502019258948351, 406.9948905683720000, 15.47720386886985189 ) ) ;
#14210 = EDGE_CURVE ( 'NONE', #18850, #14441, #6007, .T. ) ;
#14211 = CARTESIAN_POINT ( 'NONE',  ( -14.54375231895776821, 338.2448905765656377, -14.14213562373094746 ) ) ;
#14212 = DIRECTION ( 'NONE',  ( -0.000000000000000000, -1.000000000000000000, -0.000000000000000000 ) ) ;
#14213 = CARTESIAN_POINT ( 'NONE',  ( -44.16309181155855867, 304.4948905683720568, 6.410867750099241924 ) ) ;
#14214 = CARTESIAN_POINT ( 'NONE',  ( -13.20868407381887089, 459.7448905683720568, 6.410867750099229490 ) ) ;
#14215 = DIRECTION ( 'NONE',  ( 0.000000000000000000, 0.000000000000000000, -1.000000000000000000 ) ) ;
#14216 = CARTESIAN_POINT ( 'NONE',  ( -203.6858879426887654, 610.7448905601785327, 2.143131898507868248E-14 ) ) ;
#14217 = DIRECTION ( 'NONE',  ( 0.000000000000000000, -1.000000000000000000, 0.000000000000000000 ) ) ;
#14218 = AXIS2_PLACEMENT_3D ( 'NONE', #20153, #5321, #19831 ) ;
#14219 = CARTESIAN_POINT ( 'NONE',  ( -42.88789093042843348, 376.3073905683720000, 9.489475012073736337 ) ) ;
#14220 = VECTOR ( 'NONE', #20584, 1000.000000000000114 ) ;
#14221 = CARTESIAN_POINT ( 'NONE',  ( -14.48388495494901740, 509.8073905683720000, -9.489475012073736337 ) ) ;
#14222 = CARTESIAN_POINT ( 'NONE',  ( -36.33955658999052929, 499.1198905601784759, 18.47759065022572500 ) ) ;
#14223 = CARTESIAN_POINT ( 'NONE',  ( -13.20868407381885490, 328.2448905683720000, 6.410867750099229490 ) ) ;
#14224 = ADVANCED_FACE ( 'NONE', ( #4599, #17892 ), #14675, .F. ) ;
#14225 = ORIENTED_EDGE ( 'NONE', *, *, #7618, .F. ) ;
#14226 = CARTESIAN_POINT ( 'NONE',  ( -22.27502019258949417, 496.9948905683720568, 15.47720386886985189 ) ) ;
#14227 = ORIENTED_EDGE ( 'NONE', *, *, #17681, .F. ) ;
#14228 = CARTESIAN_POINT ( 'NONE',  ( -48.68588794268870146, 311.9948905765655809, 0.000000000000000000 ) ) ;
#14229 = CARTESIAN_POINT ( 'NONE',  ( -40.53162694259544452, 424.1198905683720000, -11.84573899990672707 ) ) ;
#14230 = CARTESIAN_POINT ( 'NONE',  ( -8.685887942688859553, 396.6823905765656377, 3.978247347593479866 ) ) ;
#14231 = DIRECTION ( 'NONE',  ( 0.000000000000000000, 1.000000000000000000, 0.000000000000000000 ) ) ;
#14232 = CARTESIAN_POINT ( 'NONE',  ( -14.48388495494901385, 469.8073905683719431, -9.489475012073736337 ) ) ;
#14233 = ORIENTED_EDGE ( 'NONE', *, *, #16114, .F. ) ;
#14234 = CARTESIAN_POINT ( 'NONE',  ( -19.19641293061498999, 457.3073905683720568, 14.20200298773971426 ) ) ;
#14235 = CARTESIAN_POINT ( 'NONE',  ( -48.68588794268878672, 242.3073905765656093, 3.978247347592954952 ) ) ;
#14236 = EDGE_CURVE ( 'NONE', #3567, #18006, #8860, .T. ) ;
#14237 = CARTESIAN_POINT ( 'NONE',  ( -42.82802356641966668, 400.7448905765656377, -14.14213562373094746 ) ) ;
#14238 = CARTESIAN_POINT ( 'NONE',  ( -17.35679799567828496, 278.5573905765656377, -16.95518130045146421 ) ) ;
#14239=STYLED_ITEM('',(#21414),#11152);
#14240 = CARTESIAN_POINT ( 'NONE',  ( -21.03221929538692336, 368.8698905765656377, -18.47759065022572855 ) ) ;
#14241 = DIRECTION ( 'NONE',  ( -1.000000000000000000, -0.000000000000000000, -0.000000000000000000 ) ) ;
#14242 = FACE_OUTER_BOUND ( 'NONE', #4422, .T. ) ;
#14243 = DIRECTION ( 'NONE',  ( 0.000000000000000000, 1.000000000000000000, -0.000000000000000000 ) ) ;
#14244 = DIRECTION ( 'NONE',  ( 0.000000000000000000, 0.000000000000000000, 1.000000000000000000 ) ) ;
#14245 = DIRECTION ( 'NONE',  ( -0.000000000000000000, -0.000000000000000000, 1.000000000000000000 ) ) ;
#14246 = CARTESIAN_POINT ( 'NONE',  ( -10.20829729246297291, 242.8698905601785043, -7.653668647301794969 ) ) ;
#14247 = B_SPLINE_CURVE_WITH_KNOTS ( 'NONE', 3,
 ( #18789, #17397, #10670, #15460, #17186, #10563, #20856, #7534 ),
 .UNSPECIFIED., .F., .F.,
 ( 4, 2, 2, 4 ),
 ( 0.003797433802554437202, 0.004743183970586235289, 0.005688934138618033376, 0.007580434474681629550 ),
 .UNSPECIFIED. ) ;
#14248 = FACE_OUTER_BOUND ( 'NONE', #680, .T. ) ;
#14249 = CARTESIAN_POINT ( 'NONE',  ( -38.17536295476245556, 436.9323905683720568, 14.20200298773971781 ) ) ;
#14250 = CARTESIAN_POINT ( 'NONE',  ( -8.685887942688738761, 502.2448905601784190, -2.449293598294705724E-15 ) ) ;
#14251 = CARTESIAN_POINT ( 'NONE',  ( -42.88789093042841927, 244.4323905683720284, -9.489475012073736337 ) ) ;
#14252 = ORIENTED_EDGE ( 'NONE', *, *, #8610, .T. ) ;
#14253 = EDGE_LOOP ( 'NONE', ( #8584, #16955 ) ) ;
#14254 = DIRECTION ( 'NONE',  ( -1.191790137725560488E-16, 1.000000000000000000, -0.000000000000000000 ) ) ;
#14255 = VERTEX_POINT ( 'NONE', #2775 ) ;
#14256 = CARTESIAN_POINT ( 'NONE',  ( -16.84014894278200103, 461.6198905683720568, -11.84573899990672707 ) ) ;
#14257 = COLOUR_RGB ( '',0.7921568627450980005, 0.8196078431372548767, 0.9333333333333333481 ) ;
#14258 = ORIENTED_EDGE ( 'NONE', *, *, #2446, .F. ) ;
#14259 = FACE_OUTER_BOUND ( 'NONE', #7733, .T. ) ;
#14260 = CARTESIAN_POINT ( 'NONE',  ( -44.16309181155855157, 244.4948905683720284, 6.410867750099241924 ) ) ;
#14261 = ORIENTED_EDGE ( 'NONE', *, *, #16587, .T. ) ;
#14262 = CARTESIAN_POINT ( 'NONE',  ( -22.27502019258949417, 516.9948905683720568, 15.47720386886985189 ) ) ;
#14263 = DIRECTION ( 'NONE',  ( 0.000000000000000000, -0.8660254037844381525, -0.5000000000000009992 ) ) ;
#14264 = CARTESIAN_POINT ( 'NONE',  ( -42.82802356641967378, 470.7448905765655809, -14.14213562373094746 ) ) ;
#14265 = DIRECTION ( 'NONE',  ( 0.000000000000000000, -0.000000000000000000, 1.000000000000000000 ) ) ;
#14266 = CARTESIAN_POINT ( 'NONE',  ( -24.70764059509554045, 284.8073905765656377, 19.99999999999998934 ) ) ;
#14267 = CARTESIAN_POINT ( 'NONE',  ( -18.66797547166049753, 223.9102039777116602, -17.31025331282116397 ) ) ;
#14268 = EDGE_CURVE ( 'NONE', #5663, #2119, #12674, .T. ) ;
#14269 = FACE_OUTER_BOUND ( 'NONE', #7141, .T. ) ;
#14270 = CIRCLE ( 'NONE', #803, 175.0000000000000284 ) ;
#14271 = EDGE_CURVE ( 'NONE', #4211, #2296, #2984, .T. ) ;
#14272 = DIRECTION ( 'NONE',  ( 1.000000000000000000, 0.000000000000000000, 0.000000000000000000 ) ) ;
#14273 = CARTESIAN_POINT ( 'NONE',  ( -16.84014894278197616, 230.1198905683720000, -11.84573899990672707 ) ) ;
#14274 =( BOUNDED_CURVE ( )  B_SPLINE_CURVE ( 2, ( #8166, #21168, #21381, #11536, #9484, #18128, #17706, #9795, #2903, #16094, #6340, #9588, #12952, #21271, #16314, #19542, #1486 ),
 .UNSPECIFIED., .F., .T. ) 
 B_SPLINE_CURVE_WITH_KNOTS ( ( 3, 2, 2, 2, 2, 2, 2, 2, 3 ),
 ( 0.7656250000000001110, 0.7675781250000001110, 0.7695312500000001110, 0.7714843750000001110, 0.7734375000000001110, 0.7753906250000001110, 0.7773437500000001110, 0.7792968750000001110, 0.7812500000000001110 ),
 .UNSPECIFIED. ) 
 CURVE ( )  GEOMETRIC_REPRESENTATION_ITEM ( )  RATIONAL_B_SPLINE_CURVE ( ( 0.9999999999999988898, 0.9807852804032315408, 1.000000000000000000, 0.9807852804032304306, 1.000000000000000000, 0.9807852804032304306, 1.000000000000000000, 0.9807852804032304306, 1.000000000000000000, 0.9807852804032304306, 1.000000000000000000, 0.9807852804032304306, 1.000000000000000000, 0.9807852804032304306, 1.000000000000000000, 0.9807852804032293204, 1.000000000000001110 ) ) 
 REPRESENTATION_ITEM ( '' )  );
#14275 = CARTESIAN_POINT ( 'NONE',  ( -42.88789093042843348, 334.4323905683720568, -9.489475012073736337 ) ) ;
#14276 = CARTESIAN_POINT ( 'NONE',  ( -48.68588794268872277, 467.2448905601784759, 0.000000000000000000 ) ) ;
#14277 = DIRECTION ( 'NONE',  ( -0.000000000000000000, -0.000000000000000000, 1.000000000000000000 ) ) ;
#14278 = CARTESIAN_POINT ( 'NONE',  ( -11.93348319268871549, 310.3698905683720568, -2.051577885510841163E-15 ) ) ;
#14279 = CARTESIAN_POINT ( 'NONE',  ( -22.27502019258949062, 380.7448905683720000, -15.47720386886985544 ) ) ;
#14280 = LINE ( 'NONE', #4089, #2910 ) ;
#14281 = APPLICATION_CONTEXT ( 'automotive_design' ) ;
#14282 = VECTOR ( 'NONE', #2394, 1000.000000000000000 ) ;
#14283 = CARTESIAN_POINT ( 'NONE',  ( -17.35679799567829562, 390.6823905601785327, 16.95518130045146421 ) ) ;
#14284 = CARTESIAN_POINT ( 'NONE',  ( -36.33955658999051508, 405.3698905601785327, -18.47759065022572855 ) ) ;
#14285 = EDGE_LOOP ( 'NONE', ( #240, #3306, #5991, #16692 ) ) ;
#14286 = ORIENTED_EDGE ( 'NONE', *, *, #11991, .F. ) ;
#14287 = CARTESIAN_POINT ( 'NONE',  ( -28.68588794268873343, 512.8698905683719431, -16.75240474999999307 ) ) ;
#14288 = FACE_OUTER_BOUND ( 'NONE', #17383, .T. ) ;
#14289 = EDGE_LOOP ( 'NONE', ( #6540, #1501, #657, #19367 ) ) ;
#14290 = CARTESIAN_POINT ( 'NONE',  ( -22.27502019258947996, 302.2448905683720000, -15.47720386886985544 ) ) ;
#14291 = ORIENTED_EDGE ( 'NONE', *, *, #10354, .T. ) ;
#14292 = CARTESIAN_POINT ( 'NONE',  ( -16.84014894278198682, 330.1198905683720568, -11.84573899990672707 ) ) ;
#14293 = CIRCLE ( 'NONE', #8050, 50.00000000000000000 ) ;
#14294 = CARTESIAN_POINT ( 'NONE',  ( -47.16347859291443712, 271.3698905765656377, -7.653668647301793193 ) ) ;
#14295 = CARTESIAN_POINT ( 'NONE',  ( -47.16347859291445843, 501.3698905765655809, -7.653668647301793193 ) ) ;
#14296 = CARTESIAN_POINT ( 'NONE',  ( -25.35362745456396638, 246.6823905683720568, 16.75240474999998952 ) ) ;
#14297 = CARTESIAN_POINT ( 'NONE',  ( -28.68588794268872277, 333.8848358243226357, 20.00000000000000000 ) ) ;
#14298 = AXIS2_PLACEMENT_3D ( 'NONE', #18286, #1976, #13330 ) ;
#14299 = CARTESIAN_POINT ( 'NONE',  ( -44.16309181155857999, 404.7448905683720568, -6.410867750099231266 ) ) ;
#14300 = DIRECTION ( 'NONE',  ( 0.000000000000000000, -1.000000000000000000, 0.000000000000000000 ) ) ;
#14301 = DIRECTION ( 'NONE',  ( 0.000000000000000000, 0.000000000000000000, 1.000000000000000000 ) ) ;
#14302 = CARTESIAN_POINT ( 'NONE',  ( -48.68588794268872988, 511.9948905765656377, 0.000000000000000000 ) ) ;
#14303 = CARTESIAN_POINT ( 'NONE',  ( -32.01814843081345430, 436.0573905683720568, 16.75240474999999307 ) ) ;
#14304 = ORIENTED_EDGE ( 'NONE', *, *, #15892, .F. ) ;
#14305 = CARTESIAN_POINT ( 'NONE',  ( -8.685887942688729879, 441.9323905601784759, 3.978247347593161010 ) ) ;
#14306 = CIRCLE ( 'NONE', #16729, 200.0000000000000000 ) ;
#14307 = ORIENTED_EDGE ( 'NONE', *, *, #1982, .T. ) ;
#14308 = ORIENTED_EDGE ( 'NONE', *, *, #16923, .F. ) ;
#14309 = ORIENTED_EDGE ( 'NONE', *, *, #20004, .F. ) ;
#14310 = DIRECTION ( 'NONE',  ( 1.000000000000000000, 0.000000000000000000, 0.000000000000000000 ) ) ;
#14311 = CARTESIAN_POINT ( 'NONE',  ( -10.20829729246298001, 321.6198905601784759, 7.653668647301790529 ) ) ;
#14312 = AXIS2_PLACEMENT_3D ( 'NONE', #11903, #14741, #9740 ) ;
#14313 = ADVANCED_FACE ( 'NONE', ( #2880 ), #9565, .F. ) ;
#14314 = AXIS2_PLACEMENT_3D ( 'NONE', #20744, #15886, #4304 ) ;
#14315 = CARTESIAN_POINT ( 'NONE',  ( -28.68588794268871212, 357.8698905683720568, 16.75240474999999307 ) ) ;
#14316 = CARTESIAN_POINT ( 'NONE',  ( -28.68588794268869435, 193.9102039777116602, 0.000000000000000000 ) ) ;
#14317 = EDGE_CURVE ( 'NONE', #16878, #9671, #21071, .T. ) ;
#14318 = CARTESIAN_POINT ( 'NONE',  ( -24.70764059509556887, 494.8073905765656377, 19.99999999999998934 ) ) ;
#14319 = CARTESIAN_POINT ( 'NONE',  ( -42.88789093042843348, 382.9323905683720568, -9.489475012073736337 ) ) ;
#14320 = CARTESIAN_POINT ( 'NONE',  ( -25.35362745456396638, 248.1823905683720284, 16.75240474999998952 ) ) ;
#14321 = CARTESIAN_POINT ( 'NONE',  ( -14.48388495494900674, 399.8073905683720568, -9.489475012073734561 ) ) ;
#14322 = CARTESIAN_POINT ( 'NONE',  ( -8.685887942688715668, 317.3073905765656377, -3.978247347593165895 ) ) ;
#14323 = CARTESIAN_POINT ( 'NONE',  ( -17.35679799567829207, 323.8073905601784190, -16.95518130045146421 ) ) ;
#14324 = CARTESIAN_POINT ( 'NONE',  ( -45.43829269268870519, 303.8698905683720000, 0.000000000000000000 ) ) ;
#14325 = CARTESIAN_POINT ( 'NONE',  ( -11.93348319268873148, 450.0573905683719431, 3.332260488124728415 ) ) ;
#14326 = CARTESIAN_POINT ( 'NONE',  ( -48.68588794268872277, 457.2448905601784759, 0.000000000000000000 ) ) ;
#14327 = CARTESIAN_POINT ( 'NONE',  ( -14.54375231895776821, 370.9948905601784759, 14.14213562373094568 ) ) ;
#14328 = LINE ( 'NONE', #19071, #13362 ) ;
#14329 = VECTOR ( 'NONE', #14866, 1000.000000000000000 ) ;
#14330 = CARTESIAN_POINT ( 'NONE',  ( -16.84014894278198682, 359.1198905683720568, 11.84573899990672530 ) ) ;
#14331 = CARTESIAN_POINT ( 'NONE',  ( -38.17536295476246977, 502.3073905683720568, -14.20200298773971426 ) ) ;
#14332 =( BOUNDED_CURVE ( )  B_SPLINE_CURVE ( 3, ( #13944, #2362, #15565, #4191 ),
 .UNSPECIFIED., .F., .T. ) 
 B_SPLINE_CURVE_WITH_KNOTS ( ( 4, 4 ),
 ( 3.164427803482926738, 4.453488305187281782 ),
 .UNSPECIFIED. ) 
 CURVE ( )  GEOMETRIC_REPRESENTATION_ITEM ( )  RATIONAL_B_SPLINE_CURVE ( ( 1.000000000000000000, 0.8662547274802335773, 0.8662547274802335773, 1.000000000000000000 ) ) 
 REPRESENTATION_ITEM ( '' )  );
#14333 = CARTESIAN_POINT ( 'NONE',  ( -28.68588794268873343, 514.7448905601784190, -19.99999999999999289 ) ) ;
#14334 = CARTESIAN_POINT ( 'NONE',  ( -11.93348319268871727, 328.8698905683720000, -2.051577885510841163E-15 ) ) ;
#14335 = EDGE_CURVE ( 'NONE', #14726, #16087, #19845, .T. ) ;
#14336 = EDGE_LOOP ( 'NONE', ( #5284, #9258, #4118, #8324, #9118, #6333, #18271, #11439 ) ) ;
#14337 = CARTESIAN_POINT ( 'NONE',  ( -48.68588794268872988, 527.2448905601785327, 0.000000000000000000 ) ) ;
#14338 = ORIENTED_EDGE ( 'NONE', *, *, #2940, .F. ) ;
#14339 = CARTESIAN_POINT ( 'NONE',  ( -35.09675569278795138, 423.4948905683720568, -15.47720386886985544 ) ) ;
#14340 = CARTESIAN_POINT ( 'NONE',  ( -8.685887942688731655, 446.9948905765655809, -2.449293598294705724E-15 ) ) ;
#14341 = DIRECTION ( 'NONE',  ( -1.191790137725560488E-16, 1.000000000000000000, -0.000000000000000000 ) ) ;
#14342 = CARTESIAN_POINT ( 'NONE',  ( -11.93348319268873148, 449.1823905683720000, -3.332260488124732856 ) ) ;
#14343 = ORIENTED_EDGE ( 'NONE', *, *, #2217, .T. ) ;
#14344 = CARTESIAN_POINT ( 'NONE',  ( -44.16309181155857999, 474.4948905683720000, 6.410867750099241924 ) ) ;
#14345 = DIRECTION ( 'NONE',  ( 1.000000000000000000, 0.000000000000000000, 0.000000000000000000 ) ) ;
#14346 = LINE ( 'NONE', #6407, #19663 ) ;
#14347 = CARTESIAN_POINT ( 'NONE',  ( -45.64106924314019409, 411.0573905765656377, -11.32908994701042715 ) ) ;
#14348 = DIRECTION ( 'NONE',  ( 0.000000000000000000, 0.000000000000000000, -1.000000000000000000 ) ) ;
#14349 = CARTESIAN_POINT ( 'NONE',  ( -8.685887942688546914, 367.3073905765656377, -3.978247347592740013 ) ) ;
#14350 = DIRECTION ( 'NONE',  ( 0.000000000000000000, 0.000000000000000000, 1.000000000000000000 ) ) ;
#14351 = CARTESIAN_POINT ( 'NONE',  ( -8.685887942688710339, 256.9948905765655809, -2.449293598294705724E-15 ) ) ;
#14352 = EDGE_CURVE ( 'NONE', #10230, #18299, #13471, .T. ) ;
#14353 = CARTESIAN_POINT ( 'NONE',  ( 52.60622592008805043, 30.52886280891152282, -151.0302712373927250 ) ) ;
#14354 = CARTESIAN_POINT ( 'NONE',  ( 20.42502041961806825, 281.1055109169419666, 20.00000000000000355 ) ) ;
#14355 = CARTESIAN_POINT ( 'NONE',  ( -17.35679799567827786, 240.6823905601784759, 16.95518130045146421 ) ) ;
#14356 = DIRECTION ( 'NONE',  ( 0.000000000000000000, 0.000000000000000000, -1.000000000000000000 ) ) ;
#14357 = CARTESIAN_POINT ( 'NONE',  ( -45.43829269268871940, 435.3698905683720000, 0.000000000000000000 ) ) ;
#14358 = DIRECTION ( 'NONE',  ( -1.000000000000000000, -0.000000000000000000, -0.000000000000000000 ) ) ;
#14359 = CARTESIAN_POINT ( 'NONE',  ( -22.27502019258946220, 258.4948905683720568, 15.47720386886985189 ) ) ;
#14360 = EDGE_CURVE ( 'NONE', #10701, #10452, #11730, .T. ) ;
#14361 = VERTEX_POINT ( 'NONE', #4916 ) ;
#14362 = ORIENTED_EDGE ( 'NONE', *, *, #3929, .F. ) ;
#14363 = CARTESIAN_POINT ( 'NONE',  ( -48.68588794268873698, 573.2448905601785327, 0.000000000000000000 ) ) ;
#14364 = ORIENTED_EDGE ( 'NONE', *, *, #5380, .T. ) ;
#14365 = CARTESIAN_POINT ( 'NONE',  ( -38.17536295476246266, 456.9323905683720000, 14.20200298773971781 ) ) ;
#14366 = CARTESIAN_POINT ( 'NONE',  ( -8.685887942688706786, 226.9948905765656377, -2.449293598294705724E-15 ) ) ;
#14367 = ORIENTED_EDGE ( 'NONE', *, *, #11991, .T. ) ;
#14368 = CARTESIAN_POINT ( 'NONE',  ( -40.01497788969913927, 365.6823905601784190, -16.95518130045146421 ) ) ;
#14369 = CARTESIAN_POINT ( 'NONE',  ( -32.01814843081343298, 246.0573905683720000, 16.75240474999999307 ) ) ;
#14370 = EDGE_LOOP ( 'NONE', ( #12771, #1370, #873, #546 ) ) ;
#14371 = CARTESIAN_POINT ( 'NONE',  ( -16.84014894278201169, 530.1198905683720568, -11.84573899990672707 ) ) ;
#14372 = CARTESIAN_POINT ( 'NONE',  ( 0.05533025579362074037, 6.264553569211843254, -2.149474931388136500 ) ) ;
#14373 = CARTESIAN_POINT ( 'NONE',  ( -14.54375231895778420, 468.2448905765656377, -14.14213562373094746 ) ) ;
#14374 = DIRECTION ( 'NONE',  ( 0.000000000000000000, 0.000000000000000000, 1.000000000000000000 ) ) ;
#14375 = DIRECTION ( 'NONE',  ( -0.000000000000000000, -0.000000000000000000, 1.000000000000000000 ) ) ;
#14376 = CYLINDRICAL_SURFACE ( 'NONE', #5605, 175.0000000000000284 ) ;
#14377 = CARTESIAN_POINT ( 'NONE',  ( -39.74795651491226067, 224.0159561153923562, -12.62940942758988250 ) ) ;
#14378 = DIRECTION ( 'NONE',  ( 1.191790137725560488E-16, -1.000000000000000000, -0.000000000000000000 ) ) ;
#14379 = CARTESIAN_POINT ( 'NONE',  ( -19.19641293061497223, 230.4323905683720000, -14.20200298773971603 ) ) ;
#14380 = CARTESIAN_POINT ( 'NONE',  ( -22.27502019258947286, 318.4948905683720000, 15.47720386886985189 ) ) ;
#14381 = DIRECTION ( 'NONE',  ( -1.000000000000000000, 0.000000000000000000, -0.000000000000000000 ) ) ;
#14382 = CARTESIAN_POINT ( 'NONE',  ( 51.98438129372387806, 56.85652257517428865, -94.99999999999994316 ) ) ;
#14383 = CARTESIAN_POINT ( 'NONE',  ( -16.84014894278198327, 301.6198905683720000, -11.84573899990672707 ) ) ;
#14384 = CARTESIAN_POINT ( 'NONE',  ( -14.48388495494899963, 377.9323905683720000, 9.489475012073732785 ) ) ;
#14385 = CARTESIAN_POINT ( 'NONE',  ( -11.93348319268874036, 520.3698905683720568, -2.051577885510841163E-15 ) ) ;
#14386 = EDGE_CURVE ( 'NONE', #3879, #19682, #3304, .T. ) ;
#14387 = CARTESIAN_POINT ( 'NONE',  ( -14.54375231895776999, 390.9948905601784759, 14.14213562373094568 ) ) ;
#14388 = CARTESIAN_POINT ( 'NONE',  ( -42.82802356641964536, 230.7448905765656093, -14.14213562373094746 ) ) ;
#14389 = ORIENTED_EDGE ( 'NONE', *, *, #4601, .T. ) ;
#14390 = ORIENTED_EDGE ( 'NONE', *, *, #1749, .T. ) ;
#14391 = CARTESIAN_POINT ( 'NONE',  ( -28.68588794268873343, 492.8698905683720568, -16.75240474999999307 ) ) ;
#14392 = DIRECTION ( 'NONE',  ( -0.000000000000000000, -0.000000000000000000, -1.000000000000000000 ) ) ;
#14393 = EDGE_LOOP ( 'NONE', ( #1418, #11967, #12601, #336, #11064, #16185 ) ) ;
#14394 = CARTESIAN_POINT ( 'NONE',  ( -38.17536295476244845, 313.8073905683720000, -14.20200298773971426 ) ) ;
#14395 = CARTESIAN_POINT ( 'NONE',  ( -16.84014894278198682, 320.1198905683720568, -11.84573899990672707 ) ) ;
#14396 =( BOUNDED_CURVE ( )  B_SPLINE_CURVE ( 2, ( #18304, #8457, #6731, #6834, #13450, #1557, #5218, #16488, #11817, #5112, #16701, #14760, #47, #3600, #15186, #21344, #19934 ),
 .UNSPECIFIED., .F., .T. ) 
 B_SPLINE_CURVE_WITH_KNOTS ( ( 3, 2, 2, 2, 2, 2, 2, 2, 3 ),
 ( 0.1718750000000001665, 0.1738281250000001665, 0.1757812500000001665, 0.1777343750000001665, 0.1796875000000001665, 0.1816406250000001665, 0.1835937500000001665, 0.1855468750000001665, 0.1875000000000001665 ),
 .UNSPECIFIED. ) 
 CURVE ( )  GEOMETRIC_REPRESENTATION_ITEM ( )  RATIONAL_B_SPLINE_CURVE ( ( 0.9999999999999983347, 0.9807852804032320959, 1.000000000000000000, 0.9807852804032304306, 1.000000000000000000, 0.9807852804032304306, 1.000000000000000000, 0.9807852804032304306, 1.000000000000000000, 0.9807852804032304306, 1.000000000000000000, 0.9807852804032304306, 1.000000000000000000, 0.9807852804032304306, 1.000000000000000000, 0.9807852804032287652, 1.000000000000001554 ) ) 
 REPRESENTATION_ITEM ( '' )  );
#14397 = EDGE_CURVE ( 'NONE', #11603, #14887, #10098, .T. ) ;
#14398 = CARTESIAN_POINT ( 'NONE',  ( -48.68588794268870146, 271.6823905765656946, -3.978247347593158345 ) ) ;
#14399 = CYLINDRICAL_SURFACE ( 'NONE', #2408, 9.999999999999994671 ) ;
#14400 = DIRECTION ( 'NONE',  ( 0.000000000000000000, 0.000000000000000000, 1.000000000000000000 ) ) ;
#14401 = EDGE_CURVE ( 'NONE', #9753, #19163, #19734, .T. ) ;
#14402 = CARTESIAN_POINT ( 'NONE',  ( -42.88789093042844058, 406.3073905683719431, 9.489475012073736337 ) ) ;
#14403 = EDGE_CURVE ( 'NONE', #20734, #4181, #19673, .T. ) ;
#14404 = AXIS2_PLACEMENT_3D ( 'NONE', #2209, #18528, #5655 ) ;
#14405 = CARTESIAN_POINT ( 'NONE',  ( -36.33955658999050797, 335.3698905601784759, -18.47759065022572855 ) ) ;
#14406 = DIRECTION ( 'NONE',  ( -1.191790137725560488E-16, 1.000000000000000000, -0.000000000000000000 ) ) ;
#14407 = CARTESIAN_POINT ( 'NONE',  ( -8.685887942688399477, 507.3073905765655809, -3.978247347592341221 ) ) ;
#14408 = AXIS2_PLACEMENT_3D ( 'NONE', #1877, #8446, #4388 ) ;
#14409 = CARTESIAN_POINT ( 'NONE',  ( -16.84014894278200103, 440.1198905683720568, -11.84573899990672707 ) ) ;
#14410 = DIRECTION ( 'NONE',  ( 1.000000000000000000, 0.000000000000000000, 0.000000000000000000 ) ) ;
#14411 = VERTEX_POINT ( 'NONE', #10202 ) ;
#14412 = CARTESIAN_POINT ( 'NONE',  ( -45.64106924314020119, 456.3073905601785327, -11.32908994701042715 ) ) ;
#14413 = ADVANCED_FACE ( 'NONE', ( #5132 ), #1576, .T. ) ;
#14414 = ORIENTED_EDGE ( 'NONE', *, *, #8363, .T. ) ;
#14415 = ORIENTED_EDGE ( 'NONE', *, *, #7363, .F. ) ;
#14416 = CARTESIAN_POINT ( 'NONE',  ( -20.54277306141296222, 600.7448905601785327, 49.33244044267773631 ) ) ;
#14417 = CARTESIAN_POINT ( 'NONE',  ( -11.73070664223724613, 323.1823905601784190, -11.32908994701042715 ) ) ;
#14418 = CARTESIAN_POINT ( 'NONE',  ( -8.685887942688724550, 376.9948905765655809, -2.449293598294705724E-15 ) ) ;
#14419 = CARTESIAN_POINT ( 'NONE',  ( -42.88789093042843348, 354.4323905683720568, -9.489475012073734561 ) ) ;
#14420 = VECTOR ( 'NONE', #2425, 1000.000000000000000 ) ;
#14421 = DIRECTION ( 'NONE',  ( -1.000000000000000000, 0.000000000000000000, 0.000000000000000000 ) ) ;
#14422 = CARTESIAN_POINT ( 'NONE',  ( -8.685887942688740537, 507.3073905765656377, -3.978247347593165895 ) ) ;
#14423 = CARTESIAN_POINT ( 'NONE',  ( -28.68588794268871922, 381.3698905683720568, -16.75240474999999307 ) ) ;
#14424 = FACE_OUTER_BOUND ( 'NONE', #8637, .T. ) ;
#14425 = CARTESIAN_POINT ( 'NONE',  ( -45.43829269268871940, 414.1823905683720000, 3.332260488124734632 ) ) ;
#14426 = AXIS2_PLACEMENT_3D ( 'NONE', #1152, #15862, #9560 ) ;
#14427 = CARTESIAN_POINT ( 'NONE',  ( -17.35679799567828852, 325.4323905765656946, 16.95518130045146421 ) ) ;
#14428 = CARTESIAN_POINT ( 'NONE',  ( -28.68588794268874054, 573.2448905601785327, 0.000000000000000000 ) ) ;
#14429 = CARTESIAN_POINT ( 'NONE',  ( -42.88789093042842637, 294.8073905683720000, 9.489475012073734561 ) ) ;
#14430 = CARTESIAN_POINT ( 'NONE',  ( -45.43829269268871940, 455.6823905683720000, 3.332260488124734632 ) ) ;
#14431 = CARTESIAN_POINT ( 'NONE',  ( -10.20829729246299777, 461.6198905601784759, 7.653668647301790529 ) ) ;
#14432 = CARTESIAN_POINT ( 'NONE',  ( -71.26501780185373036, 326.0737056351150613, -25.00000000000000355 ) ) ;
#14433 = CARTESIAN_POINT ( 'NONE',  ( -71.26501780185373036, 205.1437886375728965, 5.000000000000001776 ) ) ;
#14434 = CARTESIAN_POINT ( 'NONE',  ( -45.43829269268870519, 375.6823905683720000, 3.332260488124734632 ) ) ;
#14435 = CARTESIAN_POINT ( 'NONE',  ( -13.20868407381887621, 498.2448905683720000, 6.410867750099229490 ) ) ;
#14436 = CARTESIAN_POINT ( 'NONE',  ( -21.03221929538692692, 510.3698905601785896, 18.47759065022572500 ) ) ;
#14437 = CARTESIAN_POINT ( 'NONE',  ( -45.43829269268870519, 313.8698905683720000, 0.000000000000000000 ) ) ;
#14438 = AXIS2_PLACEMENT_3D ( 'NONE', #20779, #9082, #7345 ) ;
#14439 = EDGE_LOOP ( 'NONE', ( #4115, #13296, #13790, #21372 ) ) ;
#14440 = CARTESIAN_POINT ( 'NONE',  ( -14.54375231895778953, 523.4948905601785327, -14.14213562373094746 ) ) ;
#14441 = VERTEX_POINT ( 'NONE', #70 ) ;
#14442 = DIRECTION ( 'NONE',  ( 0.000000000000000000, 0.000000000000000000, -1.000000000000000000 ) ) ;
#14443 = CARTESIAN_POINT ( 'NONE',  ( -38.17536295476245556, 426.9323905683720000, 14.20200298773971781 ) ) ;
#14444 = CARTESIAN_POINT ( 'NONE',  ( -47.16347859291445133, 392.6198905765655809, 7.653668647301805628 ) ) ;
#14445 =( NAMED_UNIT ( * ) SI_UNIT ( $, .STERADIAN. ) SOLID_ANGLE_UNIT ( ) );
#14446 = CARTESIAN_POINT ( 'NONE',  ( -13.20868407381887089, 439.4948905683720568, -6.410867750099233042 ) ) ;
#14447 = VERTEX_POINT ( 'NONE', #6637 ) ;
#14448 = CARTESIAN_POINT ( 'NONE',  ( -19.19641293061499354, 467.3073905683721136, 14.20200298773971426 ) ) ;
#14449 = CARTESIAN_POINT ( 'NONE',  ( -18.68588794268873698, 281.1055109169419666, -40.00000000000000000 ) ) ;
#14450 = CARTESIAN_POINT ( 'NONE',  ( -48.68588794268871567, 391.9948905765656377, 0.000000000000000000 ) ) ;
#14451 = DIRECTION ( 'NONE',  ( 0.000000000000000000, 0.000000000000000000, 1.000000000000000000 ) ) ;
#14452 = CARTESIAN_POINT ( 'NONE',  ( -13.68588794268874054, 588.2448905601785327, 0.000000000000000000 ) ) ;
#14453 = CARTESIAN_POINT ( 'NONE',  ( 0.000000000000000000, -5.629165124598848990, -3.250000000000004441 ) ) ;
#14454 = CARTESIAN_POINT ( 'NONE',  ( -14.54375231895775400, 255.7448905765656377, 14.14213562373094568 ) ) ;
#14455 = ADVANCED_FACE ( 'NONE', ( #3511 ), #13258, .F. ) ;
#14456 = LINE ( 'NONE', #6206, #4038 ) ;
#14457 = CARTESIAN_POINT ( 'NONE',  ( -17.35679799567828141, 253.8073905601784759, -16.95518130045146421 ) ) ;
#14458 = CARTESIAN_POINT ( 'NONE',  ( -37.43746952852602305, 223.9102039777116602, 17.72958622188000533 ) ) ;
#14459 = CARTESIAN_POINT ( 'NONE',  ( -38.17536295476246266, 423.8073905683720568, -14.20200298773971426 ) ) ;
#14460 = CARTESIAN_POINT ( 'NONE',  ( 0.000000000000000000, 5.629165124598848102, 3.250000000000005329 ) ) ;
#14461 = CARTESIAN_POINT ( 'NONE',  ( -16.84014894278197616, 241.6198905683720284, -11.84573899990672707 ) ) ;
#14462 = ORIENTED_EDGE ( 'NONE', *, *, #10448, .T. ) ;
#14463 = EDGE_LOOP ( 'NONE', ( #19136, #18252, #5952, #8560 ) ) ;
#14464 = FACE_OUTER_BOUND ( 'NONE', #3460, .T. ) ;
#14465 = ORIENTED_EDGE ( 'NONE', *, *, #2217, .F. ) ;
#14466 = CARTESIAN_POINT ( 'NONE',  ( -40.53162694259545162, 466.6198905683720000, 11.84573899990672885 ) ) ;
#14467 = CARTESIAN_POINT ( 'NONE',  ( -24.70764059509553334, 234.8073905765656093, 19.99999999999998934 ) ) ;
#14468 = EDGE_CURVE ( 'NONE', #6673, #3284, #19106, .T. ) ;
#14469 = ORIENTED_EDGE ( 'NONE', *, *, #9152, .F. ) ;
#14470 = PLANE ( 'NONE',  #8990 ) ;
#14471 = CARTESIAN_POINT ( 'NONE',  ( -19.19641293061496512, 227.3073905683720000, 14.20200298773971426 ) ) ;
#14472 = VERTEX_POINT ( 'NONE', #18742 ) ;
#14473 = CARTESIAN_POINT ( 'NONE',  ( -11.93348319268874214, 529.1823905683720568, -3.332260488124732856 ) ) ;
#14474 = CYLINDRICAL_SURFACE ( 'NONE', #7903, 40.00000000000000000 ) ;
#14475 = CARTESIAN_POINT ( 'NONE',  ( -11.73070664223726034, 447.9323905765656946, -11.32908994701042715 ) ) ;
#14476 = CARTESIAN_POINT ( 'NONE',  ( -10.20829729246298356, 351.6198905601784759, 7.653668647301790529 ) ) ;
#14477 = CARTESIAN_POINT ( 'NONE',  ( 158.8141120573112630, 610.7448905601785327, 0.000000000000000000 ) ) ;
#14478 = LINE ( 'NONE', #4935, #8022 ) ;
#14479 = DIRECTION ( 'NONE',  ( -1.000000000000000000, 0.000000000000000000, 0.000000000000000000 ) ) ;
#14480 = AXIS2_PLACEMENT_3D ( 'NONE', #4820, #7949, #11416 ) ;
#14481 = EDGE_CURVE ( 'NONE', #4866, #19427, #13680, .T. ) ;
#14482 = CARTESIAN_POINT ( 'NONE',  ( -49.57497958038185715, 160.1716627696692683, -60.00000000000000000 ) ) ;
#14483 = CARTESIAN_POINT ( 'NONE',  ( -32.01814843081343298, 236.0573905683720284, 16.75240474999999307 ) ) ;
#14484 = CARTESIAN_POINT ( 'NONE',  ( -38.17536295476244135, 326.9323905683720568, 14.20200298773971781 ) ) ;
#14485 = DIRECTION ( 'NONE',  ( 1.000000000000000000, 0.000000000000000000, 0.000000000000000000 ) ) ;
#14486 = DIRECTION ( 'NONE',  ( 1.000000000000000000, 0.000000000000000000, 0.000000000000000000 ) ) ;
#14487 = CARTESIAN_POINT ( 'NONE',  ( -32.01814843081344009, 313.1823905683720000, -16.75240474999999307 ) ) ;
#14488 = CARTESIAN_POINT ( 'NONE',  ( -45.43829269268870519, 373.5573905683720568, -3.332260488124726194 ) ) ;
#14489 = CARTESIAN_POINT ( 'NONE',  ( -16.84014894278200458, 519.1198905683720568, 11.84573899990672530 ) ) ;
#14490 = CARTESIAN_POINT ( 'NONE',  ( -14.54375231895777176, 373.4948905601784759, -14.14213562373094746 ) ) ;
#14491 = AXIS2_PLACEMENT_3D ( 'NONE', #7264, #2311, #8678 ) ;
#14492 = DIRECTION ( 'NONE',  ( 0.000000000000000000, 0.000000000000000000, 1.000000000000000000 ) ) ;
#14493 = ORIENTED_EDGE ( 'NONE', *, *, #11218, .F. ) ;
#14494 = CARTESIAN_POINT ( 'NONE',  ( -28.68588794268872633, 487.8698905683720568, 16.75240474999999307 ) ) ;
#14495 = CARTESIAN_POINT ( 'NONE',  ( 79.78925230247502043, 142.5259582928263455, 20.00000000000000355 ) ) ;
#14496 = CARTESIAN_POINT ( 'NONE',  ( -44.16309181155855867, 274.4948905683720000, 6.410867750099241924 ) ) ;
#14497 = VERTEX_POINT ( 'NONE', #12368 ) ;
#14498 = CARTESIAN_POINT ( 'NONE',  ( -44.16309181155856578, 284.7448905683720568, -6.410867750099231266 ) ) ;
#14499 = CARTESIAN_POINT ( 'NONE',  ( -19.19641293061497933, 317.3073905683720000, 14.20200298773971426 ) ) ;
#14500 = CARTESIAN_POINT ( 'NONE',  ( -10.20829729246297468, 256.3698905765656377, 7.653668647301790529 ) ) ;
#14501 = CARTESIAN_POINT ( 'NONE',  ( -14.54375231895778420, 473.4948905601785327, -14.14213562373094746 ) ) ;
#14502 = CARTESIAN_POINT ( 'NONE',  ( -19.19641293061496867, 230.4323905683720000, -14.20200298773971603 ) ) ;
#14503 = CARTESIAN_POINT ( 'NONE',  ( -18.67110661049051146, 223.9107902980306619, -17.31196565581893765 ) ) ;
#14504 = CARTESIAN_POINT ( 'NONE',  ( -13.20868407381886023, 379.7448905683720000, 6.410867750099229490 ) ) ;
#14505 = CARTESIAN_POINT ( 'NONE',  ( -43.31820119254705759, 201.3816099220727835, 3.309203535948211261 ) ) ;
#14506 = DIRECTION ( 'NONE',  ( 1.000000000000000000, 0.000000000000000000, 0.000000000000000000 ) ) ;
#14507 = LINE ( 'NONE', #1308, #11512 ) ;
#14508 = CARTESIAN_POINT ( 'NONE',  ( -42.88789093042844058, 434.8073905683720568, 9.489475012073736337 ) ) ;
#14509 = DIRECTION ( 'NONE',  ( 0.000000000000000000, 1.000000000000000000, 0.000000000000000000 ) ) ;
#14510 = ORIENTED_EDGE ( 'NONE', *, *, #19182, .F. ) ;
#14511 = CARTESIAN_POINT ( 'NONE',  ( -36.33955658999052218, 429.1198905601784759, 18.47759065022572500 ) ) ;
#14512 = ORIENTED_EDGE ( 'NONE', *, *, #6445, .F. ) ;
#14513 = ORIENTED_EDGE ( 'NONE', *, *, #6988, .T. ) ;
#14514 = ORIENTED_EDGE ( 'NONE', *, *, #18995, .F. ) ;
#14515 = CARTESIAN_POINT ( 'NONE',  ( 5.074999999999999289, 3.752776749732560368, -6.499999999999999112 ) ) ;
#14516 = CARTESIAN_POINT ( 'NONE',  ( -8.685887942688715668, 322.5573905601784759, -3.978247347593165895 ) ) ;
#14517 = CARTESIAN_POINT ( 'NONE',  ( -28.68588794268874054, 573.2448905601785327, 0.000000000000000000 ) ) ;
#14518 = EDGE_CURVE ( 'NONE', #14361, #6325, #4035, .T. ) ;
#14519 = CARTESIAN_POINT ( 'NONE',  ( -32.01814843081344719, 343.1823905683721136, -16.75240474999999307 ) ) ;
#14520 = CARTESIAN_POINT ( 'NONE',  ( -40.01497788969914637, 493.5573905765655809, 16.95518130045146776 ) ) ;
#14521 = CARTESIAN_POINT ( 'NONE',  ( -14.48388495494899963, 377.9323905683720000, 9.489475012073732785 ) ) ;
#14522 = CARTESIAN_POINT ( 'NONE',  ( -40.53162694259542320, 224.1198905683720000, -11.84573899990672707 ) ) ;
#14523 = CARTESIAN_POINT ( 'NONE',  ( -25.35362745456399480, 391.0573905683720568, -16.75240474999999307 ) ) ;
#14524 = CARTESIAN_POINT ( 'NONE',  ( -48.68588794268870146, 321.6823905765656377, -3.978247347593158345 ) ) ;
#14525 = DIRECTION ( 'NONE',  ( -0.000000000000000000, -0.000000000000000000, -1.000000000000000000 ) ) ;
#14526 = CARTESIAN_POINT ( 'NONE',  ( -38.17536295476244845, 282.3073905683720000, -14.20200298773971426 ) ) ;
#14527 =( LENGTH_UNIT ( ) NAMED_UNIT ( * ) SI_UNIT ( .MILLI., .METRE. ) );
#14528 = CARTESIAN_POINT ( 'NONE',  ( -44.16309181155857999, 434.7448905683720000, -6.410867750099231266 ) ) ;
#14529 = EDGE_CURVE ( 'NONE', #2535, #12668, #20271, .T. ) ;
#14530 = CARTESIAN_POINT ( 'NONE',  ( -40.01497788969913216, 285.6823905601784759, -16.95518130045146421 ) ) ;
#14531 = CARTESIAN_POINT ( 'NONE',  ( 5.074999999999999289, 3.752776749732560368, -6.499999999999999112 ) ) ;
#14532 = LINE ( 'NONE', #15837, #11269 ) ;
#14533 = CARTESIAN_POINT ( 'NONE',  ( -44.16309181155856578, 355.9948905683720000, 6.410867750099241924 ) ) ;
#14534 = CARTESIAN_POINT ( 'NONE',  ( -28.68588794268872988, 506.3698905683720000, 16.75240474999999307 ) ) ;
#14535 = CARTESIAN_POINT ( 'NONE',  ( -10.20829729246300310, 501.6198905601785327, 7.653668647301790529 ) ) ;
#14536 = CARTESIAN_POINT ( 'NONE',  ( -45.43829269268869808, 324.1823905683720000, 3.332260488124734632 ) ) ;
#14537 = ORIENTED_EDGE ( 'NONE', *, *, #867, .F. ) ;
#14538 = AXIS2_PLACEMENT_3D ( 'NONE', #14018, #20597, #17357 ) ;
#14539 = CARTESIAN_POINT ( 'NONE',  ( 0.1061556211655316634, 4.836380039389415408, -4.623144047065555817 ) ) ;
#14540 = EDGE_LOOP ( 'NONE', ( #16758, #4955, #5239, #18354 ) ) ;
#14541 = CIRCLE ( 'NONE', #7933, 10.00000000000000533 ) ;
#14542 = CARTESIAN_POINT ( 'NONE',  ( -11.93348319268872970, 430.0573905683721136, 3.332260488124728859 ) ) ;
#14543 = CARTESIAN_POINT ( 'NONE',  ( -8.685887942688799157, 236.6823905765655809, 3.978247347593374172 ) ) ;
#14544 = SURFACE_STYLE_FILL_AREA ( #17669 ) ;
#14545 = CARTESIAN_POINT ( 'NONE',  ( -45.43829269268872650, 453.8698905683720000, 0.000000000000000000 ) ) ;
#14546 = ORIENTED_EDGE ( 'NONE', *, *, #1355, .T. ) ;
#14547 = VECTOR ( 'NONE', #9374, 1000.000000000000000 ) ;
#14548 = CARTESIAN_POINT ( 'NONE',  ( -42.88789093042844769, 454.8073905683720568, 9.489475012073734561 ) ) ;
#14549 = CARTESIAN_POINT ( 'NONE',  ( 115.7989814974898337, 142.5259582928263455, -20.00000000000000355 ) ) ;
#14550 = PRODUCT_DEFINITION_FORMATION_WITH_SPECIFIED_SOURCE ( 'ANY', '', #9583, .NOT_KNOWN. ) ;
#14551 = CARTESIAN_POINT ( 'NONE',  ( -10.20829729246298712, 377.6198905765655809, -7.653668647301794969 ) ) ;
#14552 = CARTESIAN_POINT ( 'NONE',  ( -15.91779735428318787, 47.19211360595399896, 47.93839540604061256 ) ) ;
#14553 = DIRECTION ( 'NONE',  ( 0.000000000000000000, 1.000000000000000000, 0.000000000000000000 ) ) ;
#14554 = DIRECTION ( 'NONE',  ( -9.855701800883827197E-17, 1.000000000000000000, 0.000000000000000000 ) ) ;
#14555 = DIRECTION ( 'NONE',  ( -1.000000000000000000, 0.000000000000000000, 0.000000000000000000 ) ) ;
#14556 = CARTESIAN_POINT ( 'NONE',  ( -45.43829269268872650, 515.6823905683720568, 3.332260488124734632 ) ) ;
#14557 = CIRCLE ( 'NONE', #10039, 4.000000000000003553 ) ;
#14558 = FACE_OUTER_BOUND ( 'NONE', #961, .T. ) ;
#14559 = VECTOR ( 'NONE', #21226, 1000.000000000000000 ) ;
#14560 = CARTESIAN_POINT ( 'NONE',  ( -8.685887942688708563, 252.2448905601784475, -2.449293598294705724E-15 ) ) ;
#14561 = CARTESIAN_POINT ( 'NONE',  ( -41.47555434389672513, 223.9102039777117739, 14.04716863791190917 ) ) ;
#14562 = CARTESIAN_POINT ( 'NONE',  ( -11.93348319268872615, 410.6823905683720000, -3.332260488124732856 ) ) ;
#14563 = LINE ( 'NONE', #19625, #10246 ) ;
#14564 = CARTESIAN_POINT ( 'NONE',  ( -19.19641293061496867, 258.8073905683720000, 14.20200298773971426 ) ) ;
#14565 = ORIENTED_EDGE ( 'NONE', *, *, #9538, .T. ) ;
#14566 = ORIENTED_EDGE ( 'NONE', *, *, #6009, .F. ) ;
#14567 = DIRECTION ( 'NONE',  ( 0.1337298367054296222, -0.9910178256594273094, 0.000000000000000000 ) ) ;
#14568 = EDGE_LOOP ( 'NONE', ( #15556, #14831, #2638 ) ) ;
#14569 = CARTESIAN_POINT ( 'NONE',  ( -45.43829269268872650, 455.6823905683720000, 3.332260488124734632 ) ) ;
#14570 = CARTESIAN_POINT ( 'NONE',  ( -28.68588794268870146, 229.4948905765656377, -19.99999999999999289 ) ) ;
#14571 = EDGE_LOOP ( 'NONE', ( #7013, #16830 ) ) ;
#14572 = VECTOR ( 'NONE', #14392, 1000.000000000000000 ) ;
#14573 = DIRECTION ( 'NONE',  ( -1.191790137725560488E-16, 1.000000000000000000, -0.000000000000000000 ) ) ;
#14574 = CARTESIAN_POINT ( 'NONE',  ( -38.17536295476244135, 222.3073905683720284, -14.20200298773971426 ) ) ;
#14575 = EDGE_LOOP ( 'NONE', ( #20941, #7714, #18912 ) ) ;
#14576 = CARTESIAN_POINT ( 'NONE',  ( -44.16309181155859420, 523.2448905683719431, -6.410867750099231266 ) ) ;
#14577 = FACE_OUTER_BOUND ( 'NONE', #8149, .T. ) ;
#14578 = CARTESIAN_POINT ( 'NONE',  ( -8.685887942688731655, 446.9948905765655809, -2.449293598294705724E-15 ) ) ;
#14579 = CARTESIAN_POINT ( 'NONE',  ( 78.68120802659203150, 149.7457237375499517, 94.99999999999994316 ) ) ;
#14580 = EDGE_CURVE ( 'NONE', #18698, #1447, #596, .T. ) ;
#14581 = CARTESIAN_POINT ( 'NONE',  ( -45.43829269268871229, 354.1823905683720568, 3.332260488124734632 ) ) ;
#14582 = CARTESIAN_POINT ( 'NONE',  ( -17.35679799567829917, 455.4323905765655809, 16.95518130045146421 ) ) ;
#14583 = LINE ( 'NONE', #16202, #18051 ) ;
#14584 = CYLINDRICAL_SURFACE ( 'NONE', #16393, 4.000000000000001776 ) ;
#14585 =( BOUNDED_CURVE ( )  B_SPLINE_CURVE ( 2, ( #7951, #17909, #13053, #11418, #3106, #14582, #10007, #14692, #11534, #21166, #18126, #4822, #9900, #16631, #6338, #19972, #16312 ),
 .UNSPECIFIED., .F., .T. ) 
 B_SPLINE_CURVE_WITH_KNOTS ( ( 3, 2, 2, 2, 2, 2, 2, 2, 3 ),
 ( 0.2343750000000001943, 0.2363281250000001943, 0.2382812500000001943, 0.2402343750000001943, 0.2421875000000002220, 0.2441406250000002220, 0.2460937500000002220, 0.2480468750000002220, 0.2500000000000002220 ),
 .UNSPECIFIED. ) 
 CURVE ( )  GEOMETRIC_REPRESENTATION_ITEM ( )  RATIONAL_B_SPLINE_CURVE ( ( 0.9999999999999981126, 0.9807852804032323180, 1.000000000000000000, 0.9807852804032304306, 1.000000000000000000, 0.9807852804032304306, 1.000000000000000000, 0.9807852804032304306, 1.000000000000000000, 0.9807852804032304306, 1.000000000000000000, 0.9807852804032304306, 1.000000000000000000, 0.9807852804032304306, 1.000000000000000000, 0.9807852804032282101, 1.000000000000002220 ) ) 
 REPRESENTATION_ITEM ( '' )  );
#14586 = CYLINDRICAL_SURFACE ( 'NONE', #6275, 15.00000000000000000 ) ;
#14587 = FACE_OUTER_BOUND ( 'NONE', #3727, .T. ) ;
#14588 = CARTESIAN_POINT ( 'NONE',  ( -32.01814843081344009, 323.1823905683720000, -16.75240474999999307 ) ) ;
#14589 = FACE_OUTER_BOUND ( 'NONE', #13528, .T. ) ;
#14590 = CARTESIAN_POINT ( 'NONE',  ( -36.33955658999051508, 379.1198905601784759, 18.47759065022572500 ) ) ;
#14591 = AXIS2_PLACEMENT_3D ( 'NONE', #3442, #319, #6994 ) ;
#14592 = VECTOR ( 'NONE', #12202, 1000.000000000000000 ) ;
#14593 = CARTESIAN_POINT ( 'NONE',  ( -13.20868407381885490, 310.9948905683720568, -6.410867750099233042 ) ) ;
#14594 = CARTESIAN_POINT ( 'NONE',  ( -44.16309181155856578, 364.4948905683720568, 6.410867750099241924 ) ) ;
#14595 = CARTESIAN_POINT ( 'NONE',  ( -40.53162694259545873, 516.6198905683720568, 11.84573899990672885 ) ) ;
#14596 = CARTESIAN_POINT ( 'NONE',  ( -47.16347859291444422, 366.6198905601784759, -7.653668647301793193 ) ) ;
#14597 = EDGE_CURVE ( 'NONE', #19261, #6826, #14074, .T. ) ;
#14598 = DIRECTION ( 'NONE',  ( 1.191790137725560488E-16, -1.000000000000000000, -0.000000000000000000 ) ) ;
#14599 = ORIENTED_EDGE ( 'NONE', *, *, #2295, .T. ) ;
#14600 = CARTESIAN_POINT ( 'NONE',  ( -11.93348319268873681, 490.6823905683720568, -3.332260488124732856 ) ) ;
#14601 = CARTESIAN_POINT ( 'NONE',  ( -13.20868407381884957, 288.2448905683720000, 6.410867750099229490 ) ) ;
#14602 = ORIENTED_EDGE ( 'NONE', *, *, #3210, .T. ) ;
#14603 = CARTESIAN_POINT ( 'NONE',  ( -45.43829269268870519, 285.0573905683720568, -3.332260488124726638 ) ) ;
#14604 = CARTESIAN_POINT ( 'NONE',  ( -28.68588794268871212, 321.3698905683720568, -16.75240474999999307 ) ) ;
#14605 = TOROIDAL_SURFACE ( 'NONE', #19422, 4.400000000000000355, 0.4000000000000000222 ) ;
#14606 = CARTESIAN_POINT ( 'NONE',  ( -28.68588794268870501, 262.8698905683720000, -16.75240474999999307 ) ) ;
#14607 = CARTESIAN_POINT ( 'NONE',  ( -36.33955658999050087, 263.8698905765656377, 18.47759065022572500 ) ) ;
#14608 = FACE_OUTER_BOUND ( 'NONE', #21151, .T. ) ;
#14609 = CARTESIAN_POINT ( 'NONE',  ( 81.24038404635966515, -343.0245277843623057, 94.99999999999994316 ) ) ;
#14610 = FACE_OUTER_BOUND ( 'NONE', #6649, .T. ) ;
#14611 = CARTESIAN_POINT ( 'NONE',  ( -13.20868407381886200, 370.9948905683720568, -6.410867750099233042 ) ) ;
#14612 = EDGE_CURVE ( 'NONE', #4925, #10315, #6435, .T. ) ;
#14613 = DIRECTION ( 'NONE',  ( 0.000000000000000000, 1.000000000000000000, 0.000000000000000000 ) ) ;
#14614 = CARTESIAN_POINT ( 'NONE',  ( -47.16347859291445843, 461.3698905765656377, -7.653668647301793193 ) ) ;
#14615 = PRODUCT_DEFINITION_SHAPE ( 'NONE', 'NONE',  #21399 ) ;
#14616 = VECTOR ( 'NONE', #20086, 1000.000000000000000 ) ;
#14617 = DIRECTION ( 'NONE',  ( -0.9283449136418786551, -0.000000000000000000, -0.3717199501173604204 ) ) ;
#14618 = CARTESIAN_POINT ( 'NONE',  ( -14.48388495494900496, 419.8073905683720000, -9.489475012073736337 ) ) ;
#14619 = DIRECTION ( 'NONE',  ( -1.000000000000000000, 0.000000000000000000, 0.000000000000000000 ) ) ;
#14620 = ORIENTED_EDGE ( 'NONE', *, *, #15729, .T. ) ;
#14621 = CARTESIAN_POINT ( 'NONE',  ( -40.01497788969913927, 428.8073905601784759, 16.95518130045146776 ) ) ;
#14622 = EDGE_CURVE ( 'NONE', #12217, #12962, #19581, .T. ) ;
#14623 = EDGE_LOOP ( 'NONE', ( #13959, #1263 ) ) ;
#14624 = EDGE_LOOP ( 'NONE', ( #7457, #5000, #17639, #3466, #19296 ) ) ;
#14625 = EDGE_LOOP ( 'NONE', ( #7350, #16589, #11743, #12404 ) ) ;
#14626 = LINE ( 'NONE', #14515, #20124 ) ;
#14627 = CARTESIAN_POINT ( 'NONE',  ( -14.54375231895776466, 313.4948905601784759, -14.14213562373094746 ) ) ;
#14628 = CARTESIAN_POINT ( 'NONE',  ( -28.68588794268874054, 333.8848358243226357, -40.00000000000000000 ) ) ;
#14629 = CARTESIAN_POINT ( 'NONE',  ( -25.35362745456399125, 352.5573905683721136, -16.75240474999999307 ) ) ;
#14630 = CARTESIAN_POINT ( 'NONE',  ( -36.33955658999052929, 510.1198905765655809, -18.47759065022572855 ) ) ;
#14631 = CARTESIAN_POINT ( 'NONE',  ( -22.27502019258949062, 390.7448905683720000, -15.47720386886985544 ) ) ;
#14632 = CARTESIAN_POINT ( 'NONE',  ( -16.84014894278196905, 229.1198905683720000, 11.84573899990672530 ) ) ;
#14633 = VECTOR ( 'NONE', #18606, 1000.000000000000000 ) ;
#14634 = CARTESIAN_POINT ( 'NONE',  ( -13.20868407381886023, 378.2448905683720000, 6.410867750099229490 ) ) ;
#14635 = CARTESIAN_POINT ( 'NONE',  ( -11.73070664223724258, 326.0573905765656946, 11.32908994701042005 ) ) ;
#14636 = FACE_OUTER_BOUND ( 'NONE', #9884, .T. ) ;
#14637 = CARTESIAN_POINT ( 'NONE',  ( -42.88789093042842637, 284.8073905683720568, 9.489475012073734561 ) ) ;
#14638 =( LENGTH_UNIT ( ) NAMED_UNIT ( * ) SI_UNIT ( .MILLI., .METRE. ) );
#14639 = CARTESIAN_POINT ( 'NONE',  ( -42.88789093042844058, 444.4323905683720568, -9.489475012073736337 ) ) ;
#14640 = FACE_OUTER_BOUND ( 'NONE', #4185, .T. ) ;
#14641 = CARTESIAN_POINT ( 'NONE',  ( 35.96497763894179656, 163.7662197624121916, 60.00000000000000000 ) ) ;
#14642 = CARTESIAN_POINT ( 'NONE',  ( 146.1533239063698772, 600.7448905601785327, 7.500000000000000000 ) ) ;
#14643 = VECTOR ( 'NONE', #10075, 999.9999999999998863 ) ;
#14644 = CARTESIAN_POINT ( 'NONE',  ( -19.19641293061498288, 348.8073905683720000, 14.20200298773971426 ) ) ;
#14645 = CARTESIAN_POINT ( 'NONE',  ( -13.20868407381887444, 479.4948905683720000, -6.410867750099233042 ) ) ;
#14646 = AXIS2_PLACEMENT_3D ( 'NONE', #2548, #1150, #834 ) ;
#14647 = CARTESIAN_POINT ( 'NONE',  ( -10.20829729246299955, 482.8698905601784759, -7.653668647301794969 ) ) ;
#14648 = CARTESIAN_POINT ( 'NONE',  ( -35.09675569278794427, 315.7448905683720000, 15.47720386886985366 ) ) ;
#14649 = ORIENTED_EDGE ( 'NONE', *, *, #6915, .F. ) ;
#14650 = FACE_OUTER_BOUND ( 'NONE', #3089, .T. ) ;
#14651 = ORIENTED_EDGE ( 'NONE', *, *, #3555, .F. ) ;
#14652 = DIRECTION ( 'NONE',  ( 0.000000000000000000, 1.000000000000000000, 0.000000000000000000 ) ) ;
#14653 = ADVANCED_FACE ( 'NONE', ( #20588 ), #7273, .T. ) ;
#14654 = EDGE_CURVE ( 'NONE', #1580, #18169, #6099, .T. ) ;
#14655 = CARTESIAN_POINT ( 'NONE',  ( -11.93348319268872615, 400.3698905683720000, -2.051577885510841163E-15 ) ) ;
#14656 = CARTESIAN_POINT ( 'NONE',  ( -21.03221929538691271, 395.1198905765656377, 18.47759065022572500 ) ) ;
#14657 = DIRECTION ( 'NONE',  ( -0.000000000000000000, -0.000000000000000000, -1.000000000000000000 ) ) ;
#14658 = CARTESIAN_POINT ( 'NONE',  ( -44.16309181155857999, 443.2448905683720000, -6.410867750099231266 ) ) ;
#14659 = CARTESIAN_POINT ( 'NONE',  ( -40.53162694259544452, 445.1198905683720568, 11.84573899990672885 ) ) ;
#14660 = DIRECTION ( 'NONE',  ( 1.000000000000000000, 0.000000000000000000, 0.000000000000000000 ) ) ;
#14661 = CARTESIAN_POINT ( 'NONE',  ( -28.68588794268873698, -129.7637193493918915, 49.60091809715359545 ) ) ;
#14662 = CARTESIAN_POINT ( 'NONE',  ( -24.70764059509556532, 379.1823905765656946, -19.99999999999999289 ) ) ;
#14663 = PLANE ( 'NONE',  #14153 ) ;
#14664 = CARTESIAN_POINT ( 'NONE',  ( -24.70764059509556176, 389.1823905765656946, -19.99999999999999289 ) ) ;
#14665 = CARTESIAN_POINT ( 'NONE',  ( -28.68588794268872633, 378.8848358243226357, 0.000000000000000000 ) ) ;
#14666 = FACE_OUTER_BOUND ( 'NONE', #1137, .T. ) ;
#14667 = CIRCLE ( 'NONE', #18447, 40.00000000000000000 ) ;
#14668 = CARTESIAN_POINT ( 'NONE',  ( -19.19641293061500065, 491.9323905683720000, -14.20200298773971603 ) ) ;
#14669 = EDGE_CURVE ( 'NONE', #7864, #17482, #11937, .T. ) ;
#14670 = CARTESIAN_POINT ( 'NONE',  ( 20.42502041961813930, 230.5765313837437418, 40.00000000000000000 ) ) ;
#14671 = LINE ( 'NONE', #2770, #4180 ) ;
#14672 = CARTESIAN_POINT ( 'NONE',  ( -10.20829729246300488, 521.6198905601785327, 7.653668647301790529 ) ) ;
#14673 = EDGE_CURVE ( 'NONE', #20490, #5907, #598, .T. ) ;
#14674 = CARTESIAN_POINT ( 'NONE',  ( -45.43829269268871229, 405.6823905683720568, 3.332260488124734632 ) ) ;
#14675 = PLANE ( 'NONE',  #3682 ) ;
#14676 = CARTESIAN_POINT ( 'NONE',  ( -48.68588794268872988, 536.9323905601785327, -3.978247347593158345 ) ) ;
#14677 = EDGE_LOOP ( 'NONE', ( #7625, #7763, #13719, #13091 ) ) ;
#14678 = CARTESIAN_POINT ( 'NONE',  ( -48.68588794268880804, 422.3073905765656377, 3.978247347592954952 ) ) ;
#14679 = VERTEX_POINT ( 'NONE', #20486 ) ;
#14680 = CARTESIAN_POINT ( 'NONE',  ( -44.16309181155858710, 454.7448905683720568, -6.410867750099231266 ) ) ;
#14681 = CARTESIAN_POINT ( 'NONE',  ( -19.81322276830274731, 218.7662462910128340, -17.97266575622176532 ) ) ;
#14682 = ADVANCED_FACE ( 'NONE', ( #15628, #17346 ), #2530, .T. ) ;
#14683 = ORIENTED_EDGE ( 'NONE', *, *, #3281, .T. ) ;
#14684 = CARTESIAN_POINT ( 'NONE',  ( -43.20717515250593266, 208.4480206960199666, 3.766779594902113892 ) ) ;
#14685 = CARTESIAN_POINT ( 'NONE',  ( -28.68588794268873343, 527.8698905683720568, 16.75240474999999307 ) ) ;
#14686 = ORIENTED_EDGE ( 'NONE', *, *, #13291, .F. ) ;
#14687 = CARTESIAN_POINT ( 'NONE',  ( -19.19641293061500065, 510.4323905683720000, -14.20200298773971603 ) ) ;
#14688 = PLANE ( 'NONE',  #1366 ) ;
#14689 = CARTESIAN_POINT ( 'NONE',  ( -24.70764059509557242, 439.1823905765655809, -19.99999999999999289 ) ) ;
#14690 = CARTESIAN_POINT ( 'NONE',  ( -17.35679799567829562, 358.5573905765655809, -16.95518130045146421 ) ) ;
#14691 = DIRECTION ( 'NONE',  ( -0.000000000000000000, -0.000000000000000000, -1.000000000000000000 ) ) ;
#14692 = CARTESIAN_POINT ( 'NONE',  ( -24.70764059509555821, 454.8073905765655809, 19.99999999999998934 ) ) ;
#14693 = CARTESIAN_POINT ( 'NONE',  ( 72.94945500224395118, 285.0140030772282103, -20.00000000000000355 ) ) ;
#14694 = CARTESIAN_POINT ( 'NONE',  ( -28.68588794268874054, 573.2448905601785327, 0.000000000000000000 ) ) ;
#14695 = CARTESIAN_POINT ( 'NONE',  ( -42.88789093042841927, 234.8073905683720284, 9.489475012073736337 ) ) ;
#14696 = CARTESIAN_POINT ( 'NONE',  ( -28.68588794268870856, 312.8698905683720000, -16.75240474999999307 ) ) ;
#14697 = CARTESIAN_POINT ( 'NONE',  ( 5.299999999999999822, 3.752776749732563033, 6.500000000000000000 ) ) ;
#14698 = CARTESIAN_POINT ( 'NONE',  ( -17.35679799567827786, 260.6823905601785327, 16.95518130045146421 ) ) ;
#14699 = CYLINDRICAL_SURFACE ( 'NONE', #18885, 125.0000000000000000 ) ;
#14700 = CARTESIAN_POINT ( 'NONE',  ( -35.09675569278794427, 307.2448905683720000, 15.47720386886985366 ) ) ;
#14701 = EDGE_CURVE ( 'NONE', #19418, #7992, #16789, .T. ) ;
#14702 = CARTESIAN_POINT ( 'NONE',  ( -25.35362745456400191, 528.1823905683720568, 16.75240474999998952 ) ) ;
#14703 = CARTESIAN_POINT ( 'NONE',  ( -24.70764059509555111, 360.0573905601785327, 19.99999999999998934 ) ) ;
#14704 = CARTESIAN_POINT ( 'NONE',  ( -8.685887942688717445, 312.2448905601784759, -2.449293598294705724E-15 ) ) ;
#14705 = EDGE_LOOP ( 'NONE', ( #14364, #21045, #2146 ) ) ;
#14706 = CARTESIAN_POINT ( 'NONE',  ( -32.01814843081346140, 477.5573905683720568, 16.75240474999999307 ) ) ;
#14707 = SURFACE_SIDE_STYLE ('',( #6675 ) ) ;
#14708 = CARTESIAN_POINT ( 'NONE',  ( -25.35362745456397349, 286.6823905683720568, 16.75240474999998952 ) ) ;
#14709 = ORIENTED_EDGE ( 'NONE', *, *, #10926, .T. ) ;
#14710 =( BOUNDED_CURVE ( )  B_SPLINE_CURVE ( 2, ( #19492, #19070, #11046, #7698, #14327, #11262, #17657, #9532, #6074, #7799, #16150, #1330, #20907, #21115, #7902, #12686, #19280 ),
 .UNSPECIFIED., .F., .T. ) 
 B_SPLINE_CURVE_WITH_KNOTS ( ( 3, 2, 2, 2, 2, 2, 2, 2, 3 ),
 ( 0.5156250000000002220, 0.5175781250000002220, 0.5195312500000002220, 0.5214843750000002220, 0.5234375000000002220, 0.5253906250000003331, 0.5273437500000003331, 0.5292968750000003331, 0.5312500000000003331 ),
 .UNSPECIFIED. ) 
 CURVE ( )  GEOMETRIC_REPRESENTATION_ITEM ( )  RATIONAL_B_SPLINE_CURVE ( ( 0.9999999999999977796, 0.9807852804032326510, 1.000000000000000000, 0.9807852804032304306, 1.000000000000000000, 0.9807852804032304306, 1.000000000000000000, 0.9807852804032304306, 1.000000000000000000, 0.9807852804032304306, 1.000000000000000000, 0.9807852804032304306, 1.000000000000000000, 0.9807852804032304306, 1.000000000000000000, 0.9807852804032270999, 1.000000000000003331 ) ) 
 REPRESENTATION_ITEM ( '' )  );
#14711 = CARTESIAN_POINT ( 'NONE',  ( -35.09675569278794427, 277.2448905683720568, 15.47720386886985366 ) ) ;
#14712 = CARTESIAN_POINT ( 'NONE',  ( -32.01814843081344009, 311.6823905683720568, -16.75240474999999307 ) ) ;
#14713 = CARTESIAN_POINT ( 'NONE',  ( -17.35679799567828852, 268.5573905765656946, -16.95518130045146421 ) ) ;
#14714 = CARTESIAN_POINT ( 'NONE',  ( 72.94945500224395118, 285.0140030772282103, 40.00000000000000000 ) ) ;
#14715 = DIRECTION ( 'NONE',  ( 0.000000000000000000, -1.000000000000000000, 0.000000000000000000 ) ) ;
#14716 = CARTESIAN_POINT ( 'NONE',  ( -45.43829269268870519, 385.6823905683720000, 3.332260488124734632 ) ) ;
#14717 = EDGE_CURVE ( 'NONE', #11766, #15951, #8060, .T. ) ;
#14718 = DIRECTION ( 'NONE',  ( -1.191790137725560488E-16, 1.000000000000000000, -0.000000000000000000 ) ) ;
#14719 = CARTESIAN_POINT ( 'NONE',  ( -36.33955658999052218, 460.1198905765655809, -18.47759065022572855 ) ) ;
#14720 = CARTESIAN_POINT ( 'NONE',  ( -24.70764059509554755, 269.1823905765655809, -19.99999999999999289 ) ) ;
#14721 = CARTESIAN_POINT ( 'NONE',  ( -35.09675569278795138, 421.9948905683720000, -15.47720386886985544 ) ) ;
#14722 = FACE_OUTER_BOUND ( 'NONE', #8719, .T. ) ;
#14723 = ORIENTED_EDGE ( 'NONE', *, *, #14335, .F. ) ;
#14724 = CARTESIAN_POINT ( 'NONE',  ( -24.70764059509555821, 420.0573905601784190, 19.99999999999998934 ) ) ;
#14725 = ORIENTED_EDGE ( 'NONE', *, *, #19149, .T. ) ;
#14726 = VERTEX_POINT ( 'NONE', #18125 ) ;
#14727 = CARTESIAN_POINT ( 'NONE',  ( 0.000000000000000000, 0.000000000000000000, -60.00000000000000000 ) ) ;
#14728 = CARTESIAN_POINT ( 'NONE',  ( -10.20829729246297823, 301.6198905601784759, 7.653668647301790529 ) ) ;
#14729 = CARTESIAN_POINT ( 'NONE',  ( -42.83990393396077678, 205.8064044967071879, -4.966739033517835189 ) ) ;
#14730 = EDGE_CURVE ( 'NONE', #4363, #2506, #17863, .T. ) ;
#14731 = CARTESIAN_POINT ( 'NONE',  ( -13.20868407381885845, 340.9948905683720000, -6.410867750099233042 ) ) ;
#14732 = CARTESIAN_POINT ( 'NONE',  ( -14.54375231895778775, 508.2448905765656377, -14.14213562373094746 ) ) ;
#14733 = CARTESIAN_POINT ( 'NONE',  ( -42.88789093042843348, 374.8073905683720568, 9.489475012073736337 ) ) ;
#14734 = CARTESIAN_POINT ( 'NONE',  ( -11.93348319268870661, 230.0573905683720284, 3.332260488124728415 ) ) ;
#14735 = CARTESIAN_POINT ( 'NONE',  ( -28.68588794268871567, 386.3698905683720568, 16.75240474999999307 ) ) ;
#14736 = B_SPLINE_CURVE_WITH_KNOTS ( 'NONE', 3,
 ( #304, #198, #16742, #10120, #8495, #15121, #6872, #13491 ),
 .UNSPECIFIED., .F., .F.,
 ( 4, 2, 2, 4 ),
 ( 0.003797433802554431564, 0.004743183970586230952, 0.005688934138618030774, 0.007580434474681628683 ),
 .UNSPECIFIED. ) ;
#14737 = AXIS2_PLACEMENT_3D ( 'NONE', #5755, #12366, #5545 ) ;
#14738 = CARTESIAN_POINT ( 'NONE',  ( -48.68588794268870856, 332.3073905765655809, 3.978247347593168115 ) ) ;
#14739 = CARTESIAN_POINT ( 'NONE',  ( -28.68588794268874054, 585.7448905601785327, 0.000000000000000000 ) ) ;
#14740 = CARTESIAN_POINT ( 'NONE',  ( -45.43829269268870519, 284.1823905683720568, 3.332260488124734632 ) ) ;
#14741 = DIRECTION ( 'NONE',  ( 0.000000000000000000, -0.8660254037844381525, -0.5000000000000008882 ) ) ;
#14742 = CARTESIAN_POINT ( 'NONE',  ( -44.16309181155857289, 445.9948905683720568, 6.410867750099241924 ) ) ;
#14743 = EDGE_CURVE ( 'NONE', #1580, #10233, #3213, .T. ) ;
#14744 = AXIS2_PLACEMENT_3D ( 'NONE', #3644, #6984, #10226 ) ;
#14745 = CARTESIAN_POINT ( 'NONE',  ( -33.54679760364381025, 54.20929210266576348, 120.4143613387277867 ) ) ;
#14746 = CARTESIAN_POINT ( 'NONE',  ( -14.54375231895778420, 500.9948905601784190, 14.14213562373094568 ) ) ;
#14747 = DIRECTION ( 'NONE',  ( 0.000000000000000000, 0.000000000000000000, 1.000000000000000000 ) ) ;
#14748 = FACE_OUTER_BOUND ( 'NONE', #17638, .T. ) ;
#14749 = CARTESIAN_POINT ( 'NONE',  ( -45.43829269268870519, 345.0573905683720568, -3.332260488124726194 ) ) ;
#14750 = CARTESIAN_POINT ( 'NONE',  ( -16.84014894278200103, 487.6198905683720000, 11.84573899990672530 ) ) ;
#14751 = VERTEX_POINT ( 'NONE', #5150 ) ;
#14752 = CARTESIAN_POINT ( 'NONE',  ( -21.03221929538694113, 494.1198905601784759, -18.47759065022572855 ) ) ;
#14753 = CARTESIAN_POINT ( 'NONE',  ( -14.48388495494899253, 299.8073905683720000, -9.489475012073736337 ) ) ;
#14754 = VECTOR ( 'NONE', #9140, 1000.000000000000000 ) ;
#14755 = ORIENTED_EDGE ( 'NONE', *, *, #19444, .F. ) ;
#14756 = CARTESIAN_POINT ( 'NONE',  ( -162.2727221670389781, 10.52886280891152104, -4.999999999999990230 ) ) ;
#14757 = EDGE_LOOP ( 'NONE', ( #10180, #16858 ) ) ;
#14758 = DIRECTION ( 'NONE',  ( 0.000000000000000000, 0.000000000000000000, 1.000000000000000000 ) ) ;
#14759 = CARTESIAN_POINT ( 'NONE',  ( -45.43829269268871940, 405.0573905683721136, -3.332260488124726638 ) ) ;
#14760 = CARTESIAN_POINT ( 'NONE',  ( -40.01497788969914637, 478.8073905601785327, 16.95518130045146776 ) ) ;
#14761 = CARTESIAN_POINT ( 'NONE',  ( -11.93348319268872970, 439.1823905683720000, -3.332260488124732856 ) ) ;
#14762 = CARTESIAN_POINT ( 'NONE',  ( -19.19641293061499354, 440.4323905683720000, -14.20200298773971603 ) ) ;
#14763 = CARTESIAN_POINT ( 'NONE',  ( -48.68588794268869435, 247.2448905601785043, 0.000000000000000000 ) ) ;
#14764 = CARTESIAN_POINT ( 'NONE',  ( -21.03221929538692692, 378.8698905765656377, -18.47759065022572855 ) ) ;
#14765 = CARTESIAN_POINT ( 'NONE',  ( -24.59534672197139216, 45.54211327328065551, 49.43263578720818430 ) ) ;
#14766 = CARTESIAN_POINT ( 'NONE',  ( -8.685887942688710339, 262.2448905601784759, -2.449293598294705724E-15 ) ) ;
#14767 = CARTESIAN_POINT ( 'NONE',  ( -18.68588794268873698, 281.1055109169419666, 20.00000000000000355 ) ) ;
#14768 = LINE ( 'NONE', #8137, #18394 ) ;
#14769 = CARTESIAN_POINT ( 'NONE',  ( -28.68588794268872633, 487.8698905683720568, 16.75240474999999307 ) ) ;
#14770 = CARTESIAN_POINT ( 'NONE',  ( -28.68588794268873343, 47.23886018424757083, 49.60091809715359545 ) ) ;
#14771 = FACE_OUTER_BOUND ( 'NONE', #14463, .T. ) ;
#14772 = CARTESIAN_POINT ( 'NONE',  ( -43.20801099888741703, 208.4516271390267548, 3.763513762345671143 ) ) ;
#14773 = AXIS2_PLACEMENT_3D ( 'NONE', #6819, #5203, #16894 ) ;
#14774 = CARTESIAN_POINT ( 'NONE',  ( -44.16309181155857289, 405.9948905683720568, 6.410867750099241924 ) ) ;
#14775 = DIRECTION ( 'NONE',  ( -0.9999562017632421806, 0.000000000000000000, -0.009359196291876339252 ) ) ;
#14776 = CARTESIAN_POINT ( 'NONE',  ( -16.84014894278197616, 231.6198905683720000, -11.84573899990672707 ) ) ;
#14777 = ORIENTED_EDGE ( 'NONE', *, *, #12213, .T. ) ;
#14778 = CARTESIAN_POINT ( 'NONE',  ( 158.8141120573112630, 400.5398297725602674, 0.000000000000000000 ) ) ;
#14779 = ORIENTED_EDGE ( 'NONE', *, *, #5872, .T. ) ;
#14780 = CARTESIAN_POINT ( 'NONE',  ( -45.43829269268871940, 435.3698905683720000, 0.000000000000000000 ) ) ;
#14781 = CARTESIAN_POINT ( 'NONE',  ( -40.01497788969911795, 233.5573905765656093, 16.95518130045146776 ) ) ;
#14782 = EDGE_CURVE ( 'NONE', #18799, #3040, #20250, .T. ) ;
#14783 = CIRCLE ( 'NONE', #21331, 43.46661168214937732 ) ;
#14784 = ORIENTED_EDGE ( 'NONE', *, *, #7105, .T. ) ;
#14785 = CARTESIAN_POINT ( 'NONE',  ( 162.8695233526006803, 620.7448905601785327, -10.81142786866620575 ) ) ;
#14786 = CARTESIAN_POINT ( 'NONE',  ( -45.43829269268869808, 223.8698905683720284, 0.000000000000000000 ) ) ;
#14787 = ADVANCED_FACE ( 'NONE', ( #16630 ), #6655, .T. ) ;
#14788 = VERTEX_POINT ( 'NONE', #13277 ) ;
#14789 = CARTESIAN_POINT ( 'NONE',  ( -42.88789093042845479, 514.8073905683720568, 9.489475012073734561 ) ) ;
#14790 = EDGE_CURVE ( 'NONE', #5025, #8699, #18019, .T. ) ;
#14791 = DIRECTION ( 'NONE',  ( -1.191790137725560488E-16, 1.000000000000000000, -0.000000000000000000 ) ) ;
#14792 = EDGE_CURVE ( 'NONE', #10176, #5267, #11417, .T. ) ;
#14793 = CIRCLE ( 'NONE', #21338, 4.999999999999990230 ) ;
#14794 = CARTESIAN_POINT ( 'NONE',  ( -21.03221929538693402, 438.8698905765656377, -18.47759065022572855 ) ) ;
#14795 = LINE ( 'NONE', #14579, #19644 ) ;
#14796 = CARTESIAN_POINT ( 'NONE',  ( 79.78925230247502043, 142.5259582928263455, 40.00000000000000000 ) ) ;
#14797 = CARTESIAN_POINT ( 'NONE',  ( -8.685887942688742314, 573.2448905601785327, 2.449293598294706119E-15 ) ) ;
#14798 = CARTESIAN_POINT ( 'NONE',  ( 3.458603197740078627, 230.5765313837437418, 33.59072564020503648 ) ) ;
#14799 = FACE_OUTER_BOUND ( 'NONE', #17744, .T. ) ;
#14800 = CARTESIAN_POINT ( 'NONE',  ( -16.02813280578691391, 223.9102039777117739, 15.56881321685236763 ) ) ;
#14801 = CARTESIAN_POINT ( 'NONE',  ( -43.68588794268870146, 200.1437886375729249, -0.3330356950053358633 ) ) ;
#14802 = CARTESIAN_POINT ( 'NONE',  ( -45.43829269268869808, 325.6823905683721136, 3.332260488124734632 ) ) ;
#14803 = ADVANCED_FACE ( 'NONE', ( #3529 ), #16739, .F. ) ;
#14804 = FACE_BOUND ( 'NONE', #6423, .T. ) ;
#14805 = CARTESIAN_POINT ( 'NONE',  ( -40.01497788969911795, 268.8073905601785327, 16.95518130045146776 ) ) ;
#14806 = CARTESIAN_POINT ( 'NONE',  ( -48.68588794268870856, 341.9948905765656377, 0.000000000000000000 ) ) ;
#14807 = CARTESIAN_POINT ( 'NONE',  ( -14.48388495494898898, 289.4323905683720000, 9.489475012073732785 ) ) ;
#14808 = CARTESIAN_POINT ( 'NONE',  ( -42.88789093042845479, 524.4323905683720568, -9.489475012073734561 ) ) ;
#14809 = CARTESIAN_POINT ( 'NONE',  ( -11.73070664223724968, 371.3073905601784759, 11.32908994701042005 ) ) ;
#14810 = DIRECTION ( 'NONE',  ( -1.000000000000000000, 0.000000000000000000, 0.000000000000000000 ) ) ;
#14811 = ORIENTED_EDGE ( 'NONE', *, *, #2364, .F. ) ;
#14812 = CARTESIAN_POINT ( 'NONE',  ( -11.93348319268873503, 480.0573905683720568, 3.332260488124728415 ) ) ;
#14813 = DIRECTION ( 'NONE',  ( 0.000000000000000000, -1.000000000000000000, 0.000000000000000000 ) ) ;
#14814 = CARTESIAN_POINT ( 'NONE',  ( -45.43829269268869808, 273.5573905683720000, -3.332260488124726194 ) ) ;
#14815 = ORIENTED_EDGE ( 'NONE', *, *, #18779, .T. ) ;
#14816 = CARTESIAN_POINT ( 'NONE',  ( -71.26501780185373036, 205.1437886375728965, 0.000000000000000000 ) ) ;
#14817 = CARTESIAN_POINT ( 'NONE',  ( -44.16309181155856578, 274.7448905683720568, -6.410867750099231266 ) ) ;
#14818 = CARTESIAN_POINT ( 'NONE',  ( -38.17536295476244135, 263.8073905683720568, -14.20200298773971426 ) ) ;
#14819 = CARTESIAN_POINT ( 'NONE',  ( -17.35679799567828496, 248.5573905765656093, -16.95518130045146421 ) ) ;
#14820 = CARTESIAN_POINT ( 'NONE',  ( 6.416697501590670427, 217.7548513357008630, 45.00000000000000000 ) ) ;
#14821 = CARTESIAN_POINT ( 'NONE',  ( -40.53162694259542320, 225.1198905683720000, 11.84573899990672885 ) ) ;
#14822 = CARTESIAN_POINT ( 'NONE',  ( -28.68588794268870146, 266.3698905683720000, 16.75240474999999307 ) ) ;
#14823 = CARTESIAN_POINT ( 'NONE',  ( -14.48388495494900141, 381.3073905683720568, -9.489475012073736337 ) ) ;
#14824 = CARTESIAN_POINT ( 'NONE',  ( 28.16023193154655502, 323.8848358243226357, -20.00000000000000355 ) ) ;
#14825 = CARTESIAN_POINT ( 'NONE',  ( -8.685887942688580665, 457.3073905765655809, -3.978247347592792860 ) ) ;
#14826 = LINE ( 'NONE', #9720, #20847 ) ;
#14827 = VECTOR ( 'NONE', #18760, 1000.000000000000000 ) ;
#14828 = CARTESIAN_POINT ( 'NONE',  ( -40.53162694259544452, 432.6198905683720000, -11.84573899990672707 ) ) ;
#14829 = UNCERTAINTY_MEASURE_WITH_UNIT (LENGTH_MEASURE( 1.000000000000000082E-05 ), #16111, 'distance_accuracy_value', 'NONE');
#14830 = DIRECTION ( 'NONE',  ( -1.000000000000000000, 0.000000000000000000, 0.000000000000000000 ) ) ;
#14831 = ORIENTED_EDGE ( 'NONE', *, *, #16099, .T. ) ;
#14832 =( BOUNDED_CURVE ( )  B_SPLINE_CURVE ( 2, ( #3350, #7985, #14614, #3245, #13085, #4854, #14719, #15043, #8198, #6579, #9931, #1409, #13308, #18153, #19780, #14825, #4967 ),
 .UNSPECIFIED., .F., .T. ) 
 B_SPLINE_CURVE_WITH_KNOTS ( ( 3, 2, 2, 2, 2, 2, 2, 2, 3 ),
 ( 0.2187500000000001943, 0.2207031250000001943, 0.2226562500000001943, 0.2246093750000001943, 0.2265625000000001943, 0.2285156250000001943, 0.2304687500000001943, 0.2324218750000001943, 0.2343750000000001943 ),
 .UNSPECIFIED. ) 
 CURVE ( )  GEOMETRIC_REPRESENTATION_ITEM ( )  RATIONAL_B_SPLINE_CURVE ( ( 0.9999999999999981126, 0.9807852804032323180, 1.000000000000000000, 0.9807852804032304306, 1.000000000000000000, 0.9807852804032304306, 1.000000000000000000, 0.9807852804032304306, 1.000000000000000000, 0.9807852804032304306, 1.000000000000000000, 0.9807852804032304306, 1.000000000000000000, 0.9807852804032304306, 1.000000000000000000, 0.9807852804032285432, 1.000000000000001998 ) ) 
 REPRESENTATION_ITEM ( '' )  );
#14833 = CARTESIAN_POINT ( 'NONE',  ( -42.82802356641966668, 418.4948905601784759, 14.14213562373094923 ) ) ;
#14834 = ORIENTED_EDGE ( 'NONE', *, *, #9030, .F. ) ;
#14835 = ORIENTED_EDGE ( 'NONE', *, *, #9878, .T. ) ;
#14836 = ORIENTED_EDGE ( 'NONE', *, *, #15056, .T. ) ;
#14837 = CARTESIAN_POINT ( 'NONE',  ( -43.37409492154781532, 209.1153864038857932, -3.054836571872673101 ) ) ;
#14838 = CARTESIAN_POINT ( 'NONE',  ( -36.33955658999050797, 299.1198905601785327, 18.47759065022572500 ) ) ;
#14839 = CARTESIAN_POINT ( 'NONE',  ( -49.57497958038186425, 230.5765313837437418, -60.00000000000000000 ) ) ;
#14840 = EDGE_CURVE ( 'NONE', #10793, #2403, #18450, .T. ) ;
#14841 = CARTESIAN_POINT ( 'NONE',  ( -22.27502019258948351, 342.2448905683720568, -15.47720386886985544 ) ) ;
#14842 = CARTESIAN_POINT ( 'NONE',  ( -47.16347859291445843, 492.6198905765656377, 7.653668647301805628 ) ) ;
#14843 = CARTESIAN_POINT ( 'NONE',  ( -32.01814843081344719, 366.0573905683720000, 16.75240474999999307 ) ) ;
#14844 = CARTESIAN_POINT ( 'NONE',  ( -36.33955658999050087, 310.1198905765656377, -18.47759065022572855 ) ) ;
#14845 = APPLICATION_CONTEXT ( 'automotive_design' ) ;
#14846 = CARTESIAN_POINT ( 'NONE',  ( -45.43829269268871229, 383.8698905683720000, 0.000000000000000000 ) ) ;
#14847 = CARTESIAN_POINT ( 'NONE',  ( -47.16347859291443712, 301.3698905765655809, -7.653668647301793193 ) ) ;
#14848 = DIRECTION ( 'NONE',  ( 0.000000000000000000, 0.000000000000000000, 1.000000000000000000 ) ) ;
#14849 = EDGE_CURVE ( 'NONE', #5930, #21094, #9911, .T. ) ;
#14850 = CARTESIAN_POINT ( 'NONE',  ( -11.93348319268871016, 278.8698905683720000, -2.051577885510841163E-15 ) ) ;
#14851 = CYLINDRICAL_SURFACE ( 'NONE', #9785, 19.99999999999999645 ) ;
#14852 = CARTESIAN_POINT ( 'NONE',  ( -14.48388495494900496, 429.4323905683720000, 9.489475012073732785 ) ) ;
#14853 = CARTESIAN_POINT ( 'NONE',  ( -14.54375231895776110, 283.4948905601784759, -14.14213562373094746 ) ) ;
#14854 = CARTESIAN_POINT ( 'NONE',  ( -48.68588794268872988, 517.2448905601785327, 0.000000000000000000 ) ) ;
#14855 = DIRECTION ( 'NONE',  ( -1.000000000000000000, -0.000000000000000000, -0.000000000000000000 ) ) ;
#14856 = CARTESIAN_POINT ( 'NONE',  ( -48.68588794268871567, 447.2448905601785327, 0.000000000000000000 ) ) ;
#14857 = CARTESIAN_POINT ( 'NONE',  ( -19.19641293061497933, 338.8073905683720000, 14.20200298773971426 ) ) ;
#14858 = CARTESIAN_POINT ( 'NONE',  ( -25.35362745456399480, 486.6823905683720568, 16.75240474999998952 ) ) ;
#14859 = EDGE_LOOP ( 'NONE', ( #12342, #5875, #2040, #7525 ) ) ;
#14860 = CARTESIAN_POINT ( 'NONE',  ( -45.64106924314020119, 488.1823905601784759, 11.32908994701042715 ) ) ;
#14861 = CARTESIAN_POINT ( 'NONE',  ( -45.43829269268869808, 304.1823905683720568, 3.332260488124734632 ) ) ;
#14862 = AXIS2_PLACEMENT_3D ( 'NONE', #16972, #16762, #11880 ) ;
#14863 = ORIENTED_EDGE ( 'NONE', *, *, #5247, .F. ) ;
#14864 = PLANE ( 'NONE',  #1508 ) ;
#14865 = ORIENTED_EDGE ( 'NONE', *, *, #16102, .T. ) ;
#14866 = DIRECTION ( 'NONE',  ( -0.000000000000000000, -0.000000000000000000, 1.000000000000000000 ) ) ;
#14867 = EDGE_CURVE ( 'NONE', #9937, #3730, #1296, .T. ) ;
#14868 = CARTESIAN_POINT ( 'NONE',  ( -35.09675569278795848, 397.2448905683720568, 15.47720386886985366 ) ) ;
#14869 = CARTESIAN_POINT ( 'NONE',  ( -47.16347859291444422, 376.6198905601784759, -7.653668647301793193 ) ) ;
#14870 = CARTESIAN_POINT ( 'NONE',  ( -48.68588794268870146, 301.9948905765655809, 0.000000000000000000 ) ) ;
#14871 = CARTESIAN_POINT ( 'NONE',  ( -32.01814843081345430, 416.0573905683720568, 16.75240474999999307 ) ) ;
#14872 = CARTESIAN_POINT ( 'NONE',  ( -25.35362745456400191, 441.0573905683720000, -16.75240474999999307 ) ) ;
#14873 = CARTESIAN_POINT ( 'NONE',  ( 29.72350413846044859, 280.4463447002762564, 20.00000000000000355 ) ) ;
#14874 = CARTESIAN_POINT ( 'NONE',  ( -24.70764059509555466, 374.8073905765656377, 19.99999999999998934 ) ) ;
#14875 = CARTESIAN_POINT ( 'NONE',  ( -10.94825334483056345, 54.75396031329337632, 46.32098196382629141 ) ) ;
#14876 = CARTESIAN_POINT ( 'NONE',  ( 4.700000000000000178, 6.500000000000000888, 0.000000000000000000 ) ) ;
#14877 = CARTESIAN_POINT ( 'NONE',  ( -24.70764059509556532, 429.1823905765656946, -19.99999999999999289 ) ) ;
#14878 = CARTESIAN_POINT ( 'NONE',  ( -8.685887942688742314, 573.2448905601785327, 2.449293598294706119E-15 ) ) ;
#14879 = CARTESIAN_POINT ( 'NONE',  ( -19.19641293061500065, 501.9323905683720000, -14.20200298773971603 ) ) ;
#14880 = LINE ( 'NONE', #4695, #9903 ) ;
#14881 = CARTESIAN_POINT ( 'NONE',  ( 0.000000000000000000, 0.000000000000000000, 0.000000000000000000 ) ) ;
#14882 = CARTESIAN_POINT ( 'NONE',  ( -32.66413529028189089, 519.4323905601784190, 19.99999999999999289 ) ) ;
#14883 = EDGE_CURVE ( 'NONE', #7551, #1161, #12061, .T. ) ;
#14884 = CARTESIAN_POINT ( 'NONE',  ( -14.48388495494900496, 401.3073905683720568, -9.489475012073736337 ) ) ;
#14885 = DIRECTION ( 'NONE',  ( -1.000000000000000000, -1.191790137725560488E-16, 0.000000000000000000 ) ) ;
#14886 = CARTESIAN_POINT ( 'NONE',  ( -38.17536295476243424, 226.9323905683720000, 14.20200298773971781 ) ) ;
#14887 = VERTEX_POINT ( 'NONE', #3735 ) ;
#14888 = CARTESIAN_POINT ( 'NONE',  ( -28.68588794268872988, 516.3698905683720568, 16.75240474999999307 ) ) ;
#14889 = ORIENTED_EDGE ( 'NONE', *, *, #9276, .T. ) ;
#14890 = CARTESIAN_POINT ( 'NONE',  ( -11.93348319268873148, 450.0573905683719431, 3.332260488124728859 ) ) ;
#14891 = CARTESIAN_POINT ( 'NONE',  ( -19.19641293061500420, 520.4323905683720568, -14.20200298773971603 ) ) ;
#14892 = ADVANCED_FACE ( 'NONE', ( #8596 ), #5353, .F. ) ;
#14893 =( GEOMETRIC_REPRESENTATION_CONTEXT ( 3 ) GLOBAL_UNCERTAINTY_ASSIGNED_CONTEXT ( ( #4000 ) ) GLOBAL_UNIT_ASSIGNED_CONTEXT ( ( #7374, #914, #10836 ) ) REPRESENTATION_CONTEXT ( 'NONE', 'WORKASPACE' ) );
#14894 = CARTESIAN_POINT ( 'NONE',  ( 91.21585410611801592, 56.85652257517427444, 40.00000000000000000 ) ) ;
#14895 = CARTESIAN_POINT ( 'NONE',  ( -24.70764059509557597, 494.4323905601784190, -19.99999999999999289 ) ) ;
#14896 = CARTESIAN_POINT ( 'NONE',  ( -11.93348319268874214, 530.3698905683720568, -2.051577885510841163E-15 ) ) ;
#14897 = ORIENTED_EDGE ( 'NONE', *, *, #1250, .F. ) ;
#14898 = CARTESIAN_POINT ( 'NONE',  ( -14.48388495494901562, 499.8073905683720568, -9.489475012073734561 ) ) ;
#14899 = CARTESIAN_POINT ( 'NONE',  ( -36.33955658999052929, 489.1198905601785327, 18.47759065022572500 ) ) ;
#14900 = VECTOR ( 'NONE', #20845, 1000.000000000000114 ) ;
#14902 = VECTOR ( 'NONE', #1874, 1000.000000000000000 ) ;
#14901 = CARTESIAN_POINT ( 'NONE',  ( -48.68588794268871567, 441.9948905765656377, 0.000000000000000000 ) ) ;
#14903 = CARTESIAN_POINT ( 'NONE',  ( -8.685887942688456320, 357.3073905765655809, -3.978247347592526850 ) ) ;
#14904 = AXIS2_PLACEMENT_3D ( 'NONE', #1035, #19292, #16063 ) ;
#14905 = DIRECTION ( 'NONE',  ( -1.000000000000000000, -0.000000000000000000, -0.000000000000000000 ) ) ;
#14906 = DIRECTION ( 'NONE',  ( -1.191790137725560488E-16, 1.000000000000000000, -0.000000000000000000 ) ) ;
#14907 = CARTESIAN_POINT ( 'NONE',  ( 125.7989814974898053, 10.52886280891152104, -40.00000000000000000 ) ) ;
#14908 = CARTESIAN_POINT ( 'NONE',  ( -43.60108677734861260, 200.4027425691367057, -1.621665263882683838 ) ) ;
#14909 = CIRCLE ( 'NONE', #16618, 5.000000000000001776 ) ;
#14910 = CARTESIAN_POINT ( 'NONE',  ( -42.88789093042842637, 296.3073905683720000, 9.489475012073736337 ) ) ;
#14911 = CARTESIAN_POINT ( 'NONE',  ( -24.70764059509555111, 274.4323905601784759, -19.99999999999999289 ) ) ;
#14912 = DIRECTION ( 'NONE',  ( 0.000000000000000000, 0.000000000000000000, -1.000000000000000000 ) ) ;
#14913 = CARTESIAN_POINT ( 'NONE',  ( -14.48388495494899075, 291.3073905683720568, -9.489475012073736337 ) ) ;
#14914 = AXIS2_PLACEMENT_3D ( 'NONE', #11858, #415, #3323 ) ;
#14915 = CARTESIAN_POINT ( 'NONE',  ( -32.01814843081345430, 497.5573905683720568, 16.75240474999999307 ) ) ;
#14916 = CARTESIAN_POINT ( 'NONE',  ( -10.20829729246298534, 362.8698905601784759, -7.653668647301794969 ) ) ;
#14917 = CARTESIAN_POINT ( 'NONE',  ( -47.16347859291443712, 316.6198905601784759, -7.653668647301793193 ) ) ;
#14918 = ORIENTED_EDGE ( 'NONE', *, *, #2159, .T. ) ;
#14919 = CARTESIAN_POINT ( 'NONE',  ( -40.53162694259545162, 476.6198905683720000, 11.84573899990672885 ) ) ;
#14920 = CARTESIAN_POINT ( 'NONE',  ( -32.01814843081344009, 276.0573905683720000, 16.75240474999999307 ) ) ;
#14921 = EDGE_CURVE ( 'NONE', #10498, #19453, #16945, .T. ) ;
#14922 = VERTEX_POINT ( 'NONE', #10430 ) ;
#14923 = CARTESIAN_POINT ( 'NONE',  ( -28.68588794268874054, 573.2448905601785327, 0.000000000000000000 ) ) ;
#14924 = EDGE_CURVE ( 'NONE', #16434, #10903, #13629, .T. ) ;
#14925 = CARTESIAN_POINT ( 'NONE',  ( -44.16309181155855867, 285.9948905683720000, 6.410867750099241924 ) ) ;
#14926 = CARTESIAN_POINT ( 'NONE',  ( -40.01497788969912506, 240.4323905765656662, -16.95518130045146421 ) ) ;
#14927 = CARTESIAN_POINT ( 'NONE',  ( 82.89408817951444064, 286.0648460576640559, 40.00000000000000000 ) ) ;
#14928 = CARTESIAN_POINT ( 'NONE',  ( 118.4271928232701043, 31.85652257517428865, -40.00000000000000000 ) ) ;
#14929 = AXIS2_PLACEMENT_3D ( 'NONE', #14495, #4735, #7971 ) ;
#14930 = CARTESIAN_POINT ( 'NONE',  ( 5.299999999999999822, 3.752776749732560368, -6.499999999999999112 ) ) ;
#14931 = CARTESIAN_POINT ( 'NONE',  ( -35.09675569278794427, 275.7448905683720568, 15.47720386886985366 ) ) ;
#14932 = CARTESIAN_POINT ( 'NONE',  ( -35.09675569278795138, 387.2448905683720000, 15.47720386886985366 ) ) ;
#14933 = DIRECTION ( 'NONE',  ( 1.232945044042657126E-32, -9.855701800883825964E-17, 1.000000000000000000 ) ) ;
#14934 = CARTESIAN_POINT ( 'NONE',  ( -40.53162694259544452, 425.1198905683720000, 11.84573899990672885 ) ) ;
#14935 = CARTESIAN_POINT ( 'NONE',  ( -28.68588794268871212, 339.4948905765656377, -19.99999999999999289 ) ) ;
#14936 = ORIENTED_EDGE ( 'NONE', *, *, #16714, .T. ) ;
#14937 = CARTESIAN_POINT ( 'NONE',  ( -10.20829729246299244, 421.6198905601785327, 7.653668647301790529 ) ) ;
#14938 = VERTEX_POINT ( 'NONE', #16841 ) ;
#14939 = CARTESIAN_POINT ( 'NONE',  ( 0.5805565836007647862, 7.505553499465139389, 2.227827669841787811E-16 ) ) ;
#14940 = ORIENTED_EDGE ( 'NONE', *, *, #5344, .F. ) ;
#14941 = ORIENTED_EDGE ( 'NONE', *, *, #12793, .F. ) ;
#14942 = CARTESIAN_POINT ( 'NONE',  ( -14.48388495494901917, 531.3073905683719431, -9.489475012073736337 ) ) ;
#14943 = CARTESIAN_POINT ( 'NONE',  ( -45.64106924314017988, 308.1823905601785327, 11.32908994701042715 ) ) ;
#14944 = CARTESIAN_POINT ( 'NONE',  ( -18.68588794268873698, 323.8848358243226357, -20.00000000000000355 ) ) ;
#14945 = CARTESIAN_POINT ( 'NONE',  ( -38.17536295476245556, 343.8073905683720000, -14.20200298773971426 ) ) ;
#14946 = VERTEX_POINT ( 'NONE', #8813 ) ;
#14947 = CARTESIAN_POINT ( 'NONE',  ( -45.64106924314020119, 491.0573905765655809, -11.32908994701042715 ) ) ;
#14948 = CARTESIAN_POINT ( 'NONE',  ( -40.53162694259543741, 362.6198905683720000, -11.84573899990672707 ) ) ;
#14949 = CARTESIAN_POINT ( 'NONE',  ( -40.53162694259544452, 392.6198905683720568, -11.84573899990672707 ) ) ;
#14950 = CARTESIAN_POINT ( 'NONE',  ( -28.68588794268870856, 309.4948905765656377, -19.99999999999999289 ) ) ;
#14951 = CARTESIAN_POINT ( 'NONE',  ( -28.68588794268875475, 600.7448905601785327, 0.000000000000000000 ) ) ;
#14952 = CARTESIAN_POINT ( 'NONE',  ( -13.20868407381884779, 268.2448905683720568, 6.410867750099229490 ) ) ;
#14953 = CARTESIAN_POINT ( 'NONE',  ( -21.03221929538691981, 440.3698905601784759, 18.47759065022572500 ) ) ;
#14954 = AXIS2_PLACEMENT_3D ( 'NONE', #20930, #21034, #19200 ) ;
#14955 = CARTESIAN_POINT ( 'NONE',  ( -14.48388495494900674, 431.3073905683719431, -9.489475012073736337 ) ) ;
#14956 = CARTESIAN_POINT ( 'NONE',  ( -47.16347859291443712, 286.6198905601784759, -7.653668647301793193 ) ) ;
#14957 = CARTESIAN_POINT ( 'NONE',  ( -42.82802356641967378, 498.4948905601784759, 14.14213562373094923 ) ) ;
#14958 = CARTESIAN_POINT ( 'NONE',  ( -13.68588794268869435, 188.9102039777116602, 1.836970198721029589E-15 ) ) ;
#14959 =( BOUNDED_CURVE ( )  B_SPLINE_CURVE ( 2, ( #2025, #8268, #6760, #10317, #511, #10427, #5251, #2123, #13273, #13694, #14899, #13595, #8593, #18338, #5350, #13485, #3526 ),
 .UNSPECIFIED., .F., .T. ) 
 B_SPLINE_CURVE_WITH_KNOTS ( ( 3, 2, 2, 2, 2, 2, 2, 2, 3 ),
 ( 0.1406250000000001388, 0.1425781250000001388, 0.1445312500000001388, 0.1464843750000001388, 0.1484375000000001388, 0.1503906250000001388, 0.1523437500000001388, 0.1542968750000001388, 0.1562500000000001388 ),
 .UNSPECIFIED. ) 
 CURVE ( )  GEOMETRIC_REPRESENTATION_ITEM ( )  RATIONAL_B_SPLINE_CURVE ( ( 0.9999999999999986677, 0.9807852804032317628, 1.000000000000000000, 0.9807852804032304306, 1.000000000000000000, 0.9807852804032304306, 1.000000000000000000, 0.9807852804032304306, 1.000000000000000000, 0.9807852804032304306, 1.000000000000000000, 0.9807852804032304306, 1.000000000000000000, 0.9807852804032304306, 1.000000000000000000, 0.9807852804032290983, 1.000000000000001332 ) ) 
 REPRESENTATION_ITEM ( '' )  );
#14960 = LINE ( 'NONE', #4994, #15781 ) ;
#14961 = CARTESIAN_POINT ( 'NONE',  ( -25.35362745456399125, 352.5573905683720568, -16.75240474999999307 ) ) ;
#14962 = CARTESIAN_POINT ( 'NONE',  ( -35.09675569278795848, 481.9948905683720000, -15.47720386886985544 ) ) ;
#14963 = ORIENTED_EDGE ( 'NONE', *, *, #18010, .T. ) ;
#14964 = CARTESIAN_POINT ( 'NONE',  ( -10.20829729246300133, 491.6198905601784759, 7.653668647301790529 ) ) ;
#14965 = CARTESIAN_POINT ( 'NONE',  ( -25.35362745456397349, 296.6823905683720000, 16.75240474999998952 ) ) ;
#14966 = ORIENTED_EDGE ( 'NONE', *, *, #19532, .T. ) ;
#14967 = CARTESIAN_POINT ( 'NONE',  ( -36.33955658999051508, 343.8698905765656377, 18.47759065022572500 ) ) ;
#14968 = VERTEX_POINT ( 'NONE', #20185 ) ;
#14969 = DIRECTION ( 'NONE',  ( -1.191790137725560488E-16, 1.000000000000000000, -0.000000000000000000 ) ) ;
#14970 = APPLICATION_CONTEXT ( 'automotive_design' ) ;
#14971 = VECTOR ( 'NONE', #10593, 1000.000000000000227 ) ;
#14972 = CARTESIAN_POINT ( 'NONE',  ( -11.93348319268872615, 400.6823905683720000, -3.332260488124732856 ) ) ;
#14973 = CARTESIAN_POINT ( 'NONE',  ( -42.82802356641965957, 375.9948905601784759, -14.14213562373094746 ) ) ;
#14974 = SURFACE_STYLE_USAGE ( .BOTH. , #49 ) ;
#14975 = CARTESIAN_POINT ( 'NONE',  ( -44.16309181155857999, 423.2448905683720568, -6.410867750099231266 ) ) ;
#14976 = CARTESIAN_POINT ( 'NONE',  ( -14.48388495494898542, 259.4323905683720000, 9.489475012073732785 ) ) ;
#14977 = CARTESIAN_POINT ( 'NONE',  ( -38.17536295476246977, 452.3073905683721136, -14.20200298773971426 ) ) ;
#14978 = PRODUCT_CONTEXT ( 'NONE', #16768, 'mechanical' ) ;
#14979 = CARTESIAN_POINT ( 'NONE',  ( -28.68588794268871567, 399.7448905601784759, 19.99999999999999289 ) ) ;
#14980 = CARTESIAN_POINT ( 'NONE',  ( -40.01497788969913216, 373.5573905765655809, 16.95518130045146776 ) ) ;
#14981 = DIRECTION ( 'NONE',  ( 0.000000000000000000, -1.000000000000000000, 0.000000000000000000 ) ) ;
#14982 = DIRECTION ( 'NONE',  ( -0.9910178256594274204, -0.1337298367054296500, 0.000000000000000000 ) ) ;
#14983 = CARTESIAN_POINT ( 'NONE',  ( -48.68588794268871567, 431.9948905765656377, 0.000000000000000000 ) ) ;
#14984 = CARTESIAN_POINT ( 'NONE',  ( 4.700000000000000178, 6.500000000000000888, 0.000000000000000000 ) ) ;
#14985 = CARTESIAN_POINT ( 'NONE',  ( -16.84014894278200458, 499.1198905683720000, 11.84573899990672530 ) ) ;
#14986 = VECTOR ( 'NONE', #14598, 1000.000000000000000 ) ;
#14987 = DIRECTION ( 'NONE',  ( 0.000000000000000000, -0.000000000000000000, 1.000000000000000000 ) ) ;
#14988 = SURFACE_SIDE_STYLE ('',( #5233 ) ) ;
#14989 = CARTESIAN_POINT ( 'NONE',  ( -36.33955658999053639, 519.1198905601785327, 18.47759065022572500 ) ) ;
#14990 = VECTOR ( 'NONE', #20929, 1000.000000000000000 ) ;
#14991 = EDGE_CURVE ( 'NONE', #4497, #18564, #13697, .T. ) ;
#14992 = CARTESIAN_POINT ( 'NONE',  ( -13.20868407381886556, 400.9948905683720568, -6.410867750099233042 ) ) ;
#14993 = CARTESIAN_POINT ( 'NONE',  ( -20.54277306141296222, 600.7448905601785327, 49.33244044267773631 ) ) ;
#14994 = CARTESIAN_POINT ( 'NONE',  ( -21.25395633616651736, 222.1412455016325112, -15.05426537149049437 ) ) ;
#14995 = CARTESIAN_POINT ( 'NONE',  ( -16.84014894278199037, 370.1198905683720000, -11.84573899990672707 ) ) ;
#14996 = ORIENTED_EDGE ( 'NONE', *, *, #5260, .F. ) ;
#14997 = CARTESIAN_POINT ( 'NONE',  ( -42.88789093042845479, 524.8073905683720568, 9.489475012073736337 ) ) ;
#14998 = ORIENTED_EDGE ( 'NONE', *, *, #11658, .F. ) ;
#14999 = CARTESIAN_POINT ( 'NONE',  ( -28.68588794268872277, 447.8698905683720000, 16.75240474999999307 ) ) ;
#15000 = CARTESIAN_POINT ( 'NONE',  ( -45.43829269268873361, 523.8698905683720568, 0.000000000000000000 ) ) ;
#15001 = AXIS2_PLACEMENT_3D ( 'NONE', #19289, #2965, #12698 ) ;
#15002 = ORIENTED_EDGE ( 'NONE', *, *, #4123, .T. ) ;
#15003 = CARTESIAN_POINT ( 'NONE',  ( -45.64106924314020119, 531.0573905765656946, -11.32908994701042538 ) ) ;
#15004 = CARTESIAN_POINT ( 'NONE',  ( -32.01814843081346140, 486.0573905683721136, 16.75240474999999307 ) ) ;
#15005 = ORIENTED_EDGE ( 'NONE', *, *, #11144, .F. ) ;
#15006 = CARTESIAN_POINT ( 'NONE',  ( -32.01814843081346140, 511.6823905683719431, -16.75240474999999307 ) ) ;
#15007 = CARTESIAN_POINT ( 'NONE',  ( -12.55404211795046798, 50.68295084878040058, -46.90452445606911880 ) ) ;
#15008 = VECTOR ( 'NONE', #19643, 1000.000000000000000 ) ;
#15009 = EDGE_CURVE ( 'NONE', #3359, #10360, #20290, .T. ) ;
#15010 = CARTESIAN_POINT ( 'NONE',  ( -24.70764059509556887, 429.1823905765657514, -19.99999999999999289 ) ) ;
#15011 = CARTESIAN_POINT ( 'NONE',  ( 0.5805565836007606784, -3.752776749732561701, 6.500000000000000000 ) ) ;
#15012 = CARTESIAN_POINT ( 'NONE',  ( 81.24038404635966515, 30.52886280891152282, 94.99999999999994316 ) ) ;
#15013 = CARTESIAN_POINT ( 'NONE',  ( -1.025382690249029949, 230.5765313837437418, 25.00000000000000000 ) ) ;
#15014 = LINE ( 'NONE', #517, #11836 ) ;
#15015 = CARTESIAN_POINT ( 'NONE',  ( -33.73083959248491226, 54.96237515877132296, 49.34423148476142984 ) ) ;
#15016 = DIRECTION ( 'NONE',  ( 0.4627175328665443232, 5.514621922230504147E-17, 0.8865057725575725689 ) ) ;
#15017 = CARTESIAN_POINT ( 'NONE',  ( -43.31820119254705759, 201.3816099220727835, -3.309203535948212149 ) ) ;
#15018 = CARTESIAN_POINT ( 'NONE',  ( -14.48388495494899075, 299.4323905683720568, 9.489475012073732785 ) ) ;
#15019 = EDGE_CURVE ( 'NONE', #1471, #20916, #13916, .T. ) ;
#15020 = CARTESIAN_POINT ( 'NONE',  ( -10.20829729246300666, 531.6198905601785327, 7.653668647301790529 ) ) ;
#15021 = CARTESIAN_POINT ( 'NONE',  ( -8.685887942688710339, 262.5573905601784190, -3.978247347593165895 ) ) ;
#15022 = DIRECTION ( 'NONE',  ( -0.7071067811865511255, 0.000000000000000000, 0.7071067811865440200 ) ) ;
#15023 = AXIS2_PLACEMENT_3D ( 'NONE', #16271, #14652, #14758 ) ;
#15024 = CARTESIAN_POINT ( 'NONE',  ( -14.48388495494899075, 281.3073905683720000, -9.489475012073736337 ) ) ;
#15025 = DIRECTION ( 'NONE',  ( 1.191790137725560488E-16, -1.000000000000000000, -0.000000000000000000 ) ) ;
#15026 = CARTESIAN_POINT ( 'NONE',  ( -13.20868407381887621, 509.7448905683720000, 6.410867750099229490 ) ) ;
#15027 = DIRECTION ( 'NONE',  ( 1.000000000000000000, 0.000000000000000000, 0.000000000000000000 ) ) ;
#15028 = ORIENTED_EDGE ( 'NONE', *, *, #3138, .T. ) ;
#15029 = CARTESIAN_POINT ( 'NONE',  ( -44.16309181155858710, 474.7448905683720568, -6.410867750099231266 ) ) ;
#15030 = CARTESIAN_POINT ( 'NONE',  ( -36.33955658999051508, 410.1198905765656377, -18.47759065022572855 ) ) ;
#15031 = CARTESIAN_POINT ( 'NONE',  ( -35.09675569278793716, 265.7448905683720000, 15.47720386886985366 ) ) ;
#15032 = VERTEX_POINT ( 'NONE', #3949 ) ;
#15033 = CARTESIAN_POINT ( 'NONE',  ( 0.5805565836007715586, -7.505553499465150935, -4.964436717930768604E-16 ) ) ;
#15034 = CARTESIAN_POINT ( 'NONE',  ( -11.93348319268871016, 270.6823905683719431, -3.332260488124732856 ) ) ;
#15035 = CARTESIAN_POINT ( 'NONE',  ( -42.88789093042841927, 234.4323905683720000, -9.489475012073734561 ) ) ;
#15036 = CARTESIAN_POINT ( 'NONE',  ( -48.68588794268869435, 241.9948905765656377, 0.000000000000000000 ) ) ;
#15037 = CARTESIAN_POINT ( 'NONE',  ( -11.73070664223723902, 311.3073905601784759, 11.32908994701042005 ) ) ;
#15038 = CARTESIAN_POINT ( 'NONE',  ( -45.64106924314017277, 236.3073905601784759, -11.32908994701042715 ) ) ;
#15039 = DIRECTION ( 'NONE',  ( -1.191790137725560488E-16, 1.000000000000000000, -0.000000000000000000 ) ) ;
#15040 = CARTESIAN_POINT ( 'NONE',  ( -14.48388495494898720, 259.8073905683720000, -9.489475012073736337 ) ) ;
#15041 = CARTESIAN_POINT ( 'NONE',  ( -11.93348319268872260, 360.6823905683720568, -3.332260488124732856 ) ) ;
#15042 = CARTESIAN_POINT ( 'NONE',  ( -48.68588794268872277, 507.2448905601785327, 0.000000000000000000 ) ) ;
#15043 = CARTESIAN_POINT ( 'NONE',  ( -32.66413529028188378, 459.8073905765656946, -19.99999999999999289 ) ) ;
#15044 = EDGE_CURVE ( 'NONE', #5103, #3984, #10642, .T. ) ;
#15045 = CARTESIAN_POINT ( 'NONE',  ( -28.68588794268871922, 426.3698905683720568, 16.75240474999999307 ) ) ;
#15046 = CARTESIAN_POINT ( 'NONE',  ( -11.73070664223726389, 511.3073905601784759, 11.32908994701042005 ) ) ;
#15047 = VERTEX_POINT ( 'NONE', #10534 ) ;
#15048 = CARTESIAN_POINT ( 'NONE',  ( -10.20829729246299067, 401.6198905601784759, 7.653668647301790529 ) ) ;
#15049 = ORIENTED_EDGE ( 'NONE', *, *, #607, .T. ) ;
#15050 = VECTOR ( 'NONE', #10465, 1000.000000000000000 ) ;
#15051 = ORIENTED_EDGE ( 'NONE', *, *, #4797, .T. ) ;
#15052 = ORIENTED_EDGE ( 'NONE', *, *, #10463, .F. ) ;
#15053 = CARTESIAN_POINT ( 'NONE',  ( -14.48388495494901740, 529.4323905683720568, 9.489475012073732785 ) ) ;
#15054 = CARTESIAN_POINT ( 'NONE',  ( -8.685887942688717445, 312.2448905601784759, -2.449293598294705724E-15 ) ) ;
#15055 = FACE_OUTER_BOUND ( 'NONE', #4177, .T. ) ;
#15056 = EDGE_CURVE ( 'NONE', #8313, #16730, #8876, .T. ) ;
#15057 = CARTESIAN_POINT ( 'NONE',  ( -14.48388495494899431, 321.3073905683720568, -9.489475012073734561 ) ) ;
#15058 = CARTESIAN_POINT ( 'NONE',  ( -45.43829269268870519, 374.1823905683720568, 3.332260488124734632 ) ) ;
#15059 = ADVANCED_FACE ( 'NONE', ( #20393 ), #12282, .T. ) ;
#15060 = CARTESIAN_POINT ( 'NONE',  ( -11.93348319268872082, 358.8698905683720000, -2.051577885510841163E-15 ) ) ;
#15061 = EDGE_CURVE ( 'NONE', #1213, #16932, #13731, .T. ) ;
#15062 = CARTESIAN_POINT ( 'NONE',  ( -8.685887942688715668, 297.3073905765655809, -3.978247347593165895 ) ) ;
#15063 = DIRECTION ( 'NONE',  ( 1.000000000000000000, 0.000000000000000000, 0.000000000000000000 ) ) ;
#15064 = CARTESIAN_POINT ( 'NONE',  ( -14.48388495494898898, 269.8073905683720000, -9.489475012073734561 ) ) ;
#15065 = DIRECTION ( 'NONE',  ( 0.000000000000000000, 0.000000000000000000, 1.000000000000000000 ) ) ;
#15066 = CARTESIAN_POINT ( 'NONE',  ( -42.88789093042844058, 416.3073905683720568, 9.489475012073736337 ) ) ;
#15067 = DIRECTION ( 'NONE',  ( 1.000000000000000000, 0.000000000000000000, -0.000000000000000000 ) ) ;
#15068 = CARTESIAN_POINT ( 'NONE',  ( 0.000000000000000000, 0.000000000000000000, 6.500000000000000000 ) ) ;
#15069 = CARTESIAN_POINT ( 'NONE',  ( 71.15180554307954708, 205.5430855047783041, -43.20892846146212918 ) ) ;
#15070 = LINE ( 'NONE', #8768, #5060 ) ;
#15071 = EDGE_CURVE ( 'NONE', #10361, #10687, #17366, .T. ) ;
#15072 = CARTESIAN_POINT ( 'NONE',  ( -14.48388495494899431, 321.3073905683720000, -9.489475012073736337 ) ) ;
#15073 = CARTESIAN_POINT ( 'NONE',  ( -19.19641293061499354, 477.3073905683720568, 14.20200298773971426 ) ) ;
#15074 = ORIENTED_EDGE ( 'NONE', *, *, #8077, .F. ) ;
#15075 = CARTESIAN_POINT ( 'NONE',  ( -42.82802356641967378, 478.4948905601784759, 14.14213562373094923 ) ) ;
#15076 = CARTESIAN_POINT ( 'NONE',  ( -11.93348319268871727, 308.5573905683719431, 3.332260488124728415 ) ) ;
#15077 = VERTEX_POINT ( 'NONE', #14128 ) ;
#15078 = CARTESIAN_POINT ( 'NONE',  ( -48.68588794268887199, 342.3073905765656377, 3.978247347592742678 ) ) ;
#15079 = ORIENTED_EDGE ( 'NONE', *, *, #2280, .F. ) ;
#15080 = FACE_OUTER_BOUND ( 'NONE', #893, .T. ) ;
#15081 = CARTESIAN_POINT ( 'NONE',  ( -25.35362745456399480, 382.5573905683720000, -16.75240474999999307 ) ) ;
#15082 = CARTESIAN_POINT ( 'NONE',  ( -36.33955658999052218, 443.8698905765656377, 18.47759065022572500 ) ) ;
#15083 = CARTESIAN_POINT ( 'NONE',  ( -47.16347859291444422, 382.6198905765655809, 7.653668647301805628 ) ) ;
#15084 = CARTESIAN_POINT ( 'NONE',  ( -45.43829269268871940, 433.8698905683720568, 0.000000000000000000 ) ) ;
#15085 = CARTESIAN_POINT ( 'NONE',  ( -25.35362745456397704, 252.5573905683720284, -16.75240474999999307 ) ) ;
#15086 = CARTESIAN_POINT ( 'NONE',  ( -28.68588794268872277, 421.3698905683720568, -16.75240474999999307 ) ) ;
#15087 = APPLICATION_PROTOCOL_DEFINITION ( 'draft international standard', 'automotive_design', 1998, #16768 ) ;
#15088 = CARTESIAN_POINT ( 'NONE',  ( -17.35679799567829207, 400.6823905601784759, 16.95518130045146421 ) ) ;
#15089 = CARTESIAN_POINT ( 'NONE',  ( -11.73070664223725146, 357.9323905765656377, -11.32908994701042715 ) ) ;
#15090 = LINE ( 'NONE', #6949, #9971 ) ;
#15091 = CARTESIAN_POINT ( 'NONE',  ( -11.73070664223723725, 263.1823905601784759, -11.32908994701042538 ) ) ;
#15092 = CARTESIAN_POINT ( 'NONE',  ( -14.48388495494899431, 327.9323905683721136, 9.489475012073731008 ) ) ;
#15093 = CARTESIAN_POINT ( 'NONE',  ( 0.000000000000000000, 0.000000000000000000, 0.000000000000000000 ) ) ;
#15094 = CARTESIAN_POINT ( 'NONE',  ( -14.48388495494900852, 469.4323905683720568, 9.489475012073732785 ) ) ;
#15095 = DIRECTION ( 'NONE',  ( 0.9864615503757148129, 0.000000000000000000, -0.1639927121256943288 ) ) ;
#15096 = CARTESIAN_POINT ( 'NONE',  ( -48.68588794268872988, 527.2448905601785327, 0.000000000000000000 ) ) ;
#15097 = CARTESIAN_POINT ( 'NONE',  ( -43.68588794268869435, 210.1437886375729533, 0.1639321870911856771 ) ) ;
#15098 = CARTESIAN_POINT ( 'NONE',  ( -13.20868407381886378, 390.9948905683720568, -6.410867750099233042 ) ) ;
#15099 = DIRECTION ( 'NONE',  ( -1.000000000000000000, -0.000000000000000000, -0.000000000000000000 ) ) ;
#15100 = CARTESIAN_POINT ( 'NONE',  ( -44.16309181155855157, 225.9948905683720284, 6.410867750099241924 ) ) ;
#15101 = CARTESIAN_POINT ( 'NONE',  ( -11.93348319268872082, 358.8698905683720000, -2.051577885510841163E-15 ) ) ;
#15102 = VECTOR ( 'NONE', #2345, 1000.000000000000000 ) ;
#15103 = VERTEX_POINT ( 'NONE', #9129 ) ;
#15104 = CARTESIAN_POINT ( 'NONE',  ( -40.53162694259545873, 515.1198905683720568, 11.84573899990672885 ) ) ;
#15105 = ORIENTED_EDGE ( 'NONE', *, *, #14612, .F. ) ;
#15106 = CARTESIAN_POINT ( 'NONE',  ( -35.09675569278795848, 437.2448905683720000, 15.47720386886985366 ) ) ;
#15107 = CARTESIAN_POINT ( 'NONE',  ( -16.84014894278201169, 530.1198905683720568, -11.84573899990672707 ) ) ;
#15108 = DIRECTION ( 'NONE',  ( 1.000000000000000000, 0.000000000000000000, 0.000000000000000000 ) ) ;
#15109 = DIRECTION ( 'NONE',  ( -1.191790137725560488E-16, 1.000000000000000000, -0.000000000000000000 ) ) ;
#15110 = CARTESIAN_POINT ( 'NONE',  ( -42.88789093042844769, 482.9323905683720568, -9.489475012073736337 ) ) ;
#15111 = ORIENTED_EDGE ( 'NONE', *, *, #18476, .T. ) ;
#15112 = CARTESIAN_POINT ( 'NONE',  ( -40.53162694259545873, 512.6198905683720568, -11.84573899990672707 ) ) ;
#15113 = CARTESIAN_POINT ( 'NONE',  ( -10.76731745429010090, 56.85652257517428865, -46.25122601329427141 ) ) ;
#15114 = EDGE_CURVE ( 'NONE', #21365, #8857, #10832, .T. ) ;
#15115 = CIRCLE ( 'NONE', #261, 6.500000000000000888 ) ;
#15116 = CARTESIAN_POINT ( 'NONE',  ( -40.01497788969913927, 423.5573905765656377, 16.95518130045146776 ) ) ;
#15117 = DIRECTION ( 'NONE',  ( 0.000000000000000000, 0.000000000000000000, 1.000000000000000000 ) ) ;
#15118 = CARTESIAN_POINT ( 'NONE',  ( -48.68588794268870146, 327.2448905601785327, 0.000000000000000000 ) ) ;
#15119 = DIRECTION ( 'NONE',  ( -1.191790137725560488E-16, 1.000000000000000000, -0.000000000000000000 ) ) ;
#15120 = DIRECTION ( 'NONE',  ( -1.000000000000000000, 0.000000000000000000, 0.000000000000000000 ) ) ;
#15121 = CARTESIAN_POINT ( 'NONE',  ( 0.2578475836320759385, -6.890627091270380866, -1.065083781909174299 ) ) ;
#15122 = VECTOR ( 'NONE', #2315, 1000.000000000000114 ) ;
#15123 = LINE ( 'NONE', #5356, #19411 ) ;
#15124 = CARTESIAN_POINT ( 'NONE',  ( -9.816881303989697827, 223.9102039777117170, -6.855710153614462676 ) ) ;
#15125 = CARTESIAN_POINT ( 'NONE',  ( -11.93348319268871194, 290.3698905683720568, -2.051577885510841163E-15 ) ) ;
#15126 = CARTESIAN_POINT ( 'NONE',  ( -17.35679799567830983, 530.6823905601785327, 16.95518130045146421 ) ) ;
#15127 = CARTESIAN_POINT ( 'NONE',  ( -11.73070664223723369, 261.3073905601784759, 11.32908994701042005 ) ) ;
#15128 = FACE_OUTER_BOUND ( 'NONE', #11661, .T. ) ;
#15129 = CARTESIAN_POINT ( 'NONE',  ( -16.84014894278197971, 289.1198905683720568, 11.84573899990672530 ) ) ;
#15130 = ADVANCED_FACE ( 'NONE', ( #4589 ), #20928, .T. ) ;
#15131 = VECTOR ( 'NONE', #11827, 1000.000000000000000 ) ;
#15132 = VERTEX_POINT ( 'NONE', #4487 ) ;
#15133 = DIRECTION ( 'NONE',  ( 0.000000000000000000, 0.000000000000000000, -1.000000000000000000 ) ) ;
#15134 = CARTESIAN_POINT ( 'NONE',  ( -38.17536295476247687, 513.8073905683720568, -14.20200298773971426 ) ) ;
#15135 = VECTOR ( 'NONE', #3789, 1000.000000000000000 ) ;
#15136 = EDGE_LOOP ( 'NONE', ( #3627, #8317, #11491, #16539, #3725, #20709, #5527, #11841, #9856, #17303, #20329, #10601, #11116, #18435, #766, #19881, #3487, #12859, #18746, #18226, #11569 ) ) ;
#15137 = CARTESIAN_POINT ( 'NONE',  ( -14.48388495494900852, 459.4323905683720568, 9.489475012073732785 ) ) ;
#15138 = CARTESIAN_POINT ( 'NONE',  ( 170.2047888904039610, 620.7448905601785327, -1.893624729818132124 ) ) ;
#15139 = CARTESIAN_POINT ( 'NONE',  ( -22.27502019258947641, 260.7448905683720000, -15.47720386886985544 ) ) ;
#15140 = EDGE_LOOP ( 'NONE', ( #10256, #13373, #9171, #7169 ) ) ;
#15141 = CARTESIAN_POINT ( 'NONE',  ( -45.64106924314017988, 332.9323905765655809, 11.32908994701042538 ) ) ;
#15142 = EDGE_CURVE ( 'NONE', #454, #17590, #4377, .T. ) ;
#15143 = CARTESIAN_POINT ( 'NONE',  ( -35.09675569278793006, 253.4948905683720568, -15.47720386886985544 ) ) ;
#15144 = CARTESIAN_POINT ( 'NONE',  ( -47.16347859291443001, 241.3698905765656093, -7.653668647301793193 ) ) ;
#15145 = CARTESIAN_POINT ( 'NONE',  ( -8.685887942688717445, 312.2448905601784759, -2.449293598294705724E-15 ) ) ;
#15146 = CARTESIAN_POINT ( 'NONE',  ( -47.16347859291443001, 226.6198905601785043, -7.653668647301793193 ) ) ;
#15147 = CARTESIAN_POINT ( 'NONE',  ( -32.01814843081343298, 271.6823905683720000, -16.75240474999999307 ) ) ;
#15148 = CARTESIAN_POINT ( 'NONE',  ( -19.19641293061498288, 348.8073905683720000, 14.20200298773971426 ) ) ;
#15149 = CARTESIAN_POINT ( 'NONE',  ( -14.54375231895778775, 503.4948905601784759, -14.14213562373094746 ) ) ;
#15150 =( BOUNDED_CURVE ( )  B_SPLINE_CURVE ( 2, ( #1678, #19946, #61, #5330, #18524, #9871, #10297, #6629, #5123, #3402, #16921, #9982, #8680, #1901, #21354, #6520, #13137 ),
 .UNSPECIFIED., .F., .T. ) 
 B_SPLINE_CURVE_WITH_KNOTS ( ( 3, 2, 2, 2, 2, 2, 2, 2, 3 ),
 ( 0.1250000000000001110, 0.1269531250000001110, 0.1289062500000001110, 0.1308593750000001110, 0.1328125000000001110, 0.1347656250000001388, 0.1367187500000001388, 0.1386718750000001388, 0.1406250000000001388 ),
 .UNSPECIFIED. ) 
 CURVE ( )  GEOMETRIC_REPRESENTATION_ITEM ( )  RATIONAL_B_SPLINE_CURVE ( ( 0.9999999999999988898, 0.9807852804032315408, 1.000000000000000000, 0.9807852804032304306, 1.000000000000000000, 0.9807852804032304306, 1.000000000000000000, 0.9807852804032304306, 1.000000000000000000, 0.9807852804032304306, 1.000000000000000000, 0.9807852804032304306, 1.000000000000000000, 0.9807852804032304306, 1.000000000000000000, 0.9807852804032290983, 1.000000000000001332 ) ) 
 REPRESENTATION_ITEM ( '' )  );
#15151 = EDGE_CURVE ( 'NONE', #2675, #17585, #9574, .T. ) ;
#15152 = CARTESIAN_POINT ( 'NONE',  ( -22.27502019258948351, 406.9948905683720000, 15.47720386886985189 ) ) ;
#15153 = CARTESIAN_POINT ( 'NONE',  ( -48.68588794268878672, 507.5573905601784759, 3.978247347593009131 ) ) ;
#15154 = ORIENTED_EDGE ( 'NONE', *, *, #7561, .F. ) ;
#15155 = CARTESIAN_POINT ( 'NONE',  ( -36.33955658999052218, 409.1198905601784759, 18.47759065022572500 ) ) ;
#15156 = EDGE_LOOP ( 'NONE', ( #18161, #19660, #15589, #1742, #794, #3858 ) ) ;
#15157 = ORIENTED_EDGE ( 'NONE', *, *, #20596, .F. ) ;
#15158 = CARTESIAN_POINT ( 'NONE',  ( -11.93348319268874036, 520.6823905683719431, -3.332260488124732856 ) ) ;
#15159 = CARTESIAN_POINT ( 'NONE',  ( -21.03221929538691271, 284.1198905601784759, -18.47759065022572855 ) ) ;
#15160 = DIRECTION ( 'NONE',  ( -0.000000000000000000, -1.000000000000000000, -0.000000000000000000 ) ) ;
#15161 = CARTESIAN_POINT ( 'NONE',  ( -40.53162694259543031, 324.1198905683720568, -11.84573899990672707 ) ) ;
#15162 = CARTESIAN_POINT ( 'NONE',  ( -14.48388495494899963, 359.8073905683720000, -9.489475012073736337 ) ) ;
#15163 = CARTESIAN_POINT ( 'NONE',  ( -44.16309181155857289, 373.2448905683720000, -6.410867750099231266 ) ) ;
#15164 = CARTESIAN_POINT ( 'NONE',  ( -24.70764059509554045, 294.8073905765655809, 19.99999999999998934 ) ) ;
#15165 = DIRECTION ( 'NONE',  ( 1.000000000000000000, 0.000000000000000000, -0.000000000000000000 ) ) ;
#15166 = CARTESIAN_POINT ( 'NONE',  ( -16.84014894278197616, 257.6198905683720568, 11.84573899990672530 ) ) ;
#15167 = CARTESIAN_POINT ( 'NONE',  ( -8.685887942688820473, 441.9323905601784759, 3.978247347593374172 ) ) ;
#15168 = CARTESIAN_POINT ( 'NONE',  ( -13.20868407381886733, 420.9948905683720000, -6.410867750099233042 ) ) ;
#15169 = VECTOR ( 'NONE', #4512, 1000.000000000000000 ) ;
#15170 = CARTESIAN_POINT ( 'NONE',  ( -23.06654969220458895, 45.31613216062292082, 122.8557246090902026 ) ) ;
#15171 = LINE ( 'NONE', #13113, #20081 ) ;
#15172 = CARTESIAN_POINT ( 'NONE',  ( -10.20829729246298712, 381.6198905601784759, 7.653668647301790529 ) ) ;
#15173 = CARTESIAN_POINT ( 'NONE',  ( -33.07955326574333554, 600.7448905601785327, -10.74819839862556314 ) ) ;
#15174 = CARTESIAN_POINT ( 'NONE',  ( -45.43829269268869808, 325.6823905683721136, 3.332260488124734632 ) ) ;
#15175 = CARTESIAN_POINT ( 'NONE',  ( -35.09675569278795848, 471.9948905683720000, -15.47720386886985544 ) ) ;
#15176 = ADVANCED_FACE ( 'NONE', ( #7609 ), #6095, .T. ) ;
#15177 = VERTEX_POINT ( 'NONE', #2871 ) ;
#15178 = CARTESIAN_POINT ( 'NONE',  ( -48.68588794268872277, 457.2448905601784759, 0.000000000000000000 ) ) ;
#15179 = CARTESIAN_POINT ( 'NONE',  ( -16.84014894278197971, 297.6198905683720000, 11.84573899990672530 ) ) ;
#15180 = PLANE ( 'NONE',  #2190 ) ;
#15181 = VERTEX_POINT ( 'NONE', #12607 ) ;
#15182 = CARTESIAN_POINT ( 'NONE',  ( 20.42502041961813575, 271.1055109169419666, 40.00000000000000000 ) ) ;
#15183 = CARTESIAN_POINT ( 'NONE',  ( -8.685887942688719221, 341.9323905601785327, 3.978247347593161010 ) ) ;
#15184 = AXIS2_PLACEMENT_3D ( 'NONE', #8998, #806, #20902 ) ;
#15185 = CARTESIAN_POINT ( 'NONE',  ( -11.93348319268872260, 380.3698905683720568, -2.051577885510841163E-15 ) ) ;
#15186 = CARTESIAN_POINT ( 'NONE',  ( -47.16347859291445843, 477.8698905601784759, 7.653668647301805628 ) ) ;
#15187 = CARTESIAN_POINT ( 'NONE',  ( -22.27502019258949417, 420.7448905683720000, -15.47720386886985544 ) ) ;
#15188 = CARTESIAN_POINT ( 'NONE',  ( -35.09675569278793716, 267.2448905683720568, 15.47720386886985366 ) ) ;
#15189 = CARTESIAN_POINT ( 'NONE',  ( -44.16309181155857289, 424.4948905683720568, 6.410867750099241924 ) ) ;
#15190 = PRODUCT_CONTEXT ( 'NONE', #887, 'mechanical' ) ;
#15191 = CARTESIAN_POINT ( 'NONE',  ( -24.70764059509555111, 400.0573905601784759, 19.99999999999998934 ) ) ;
#15192 = EDGE_CURVE ( 'NONE', #21019, #18143, #3025, .T. ) ;
#15193 = CARTESIAN_POINT ( 'NONE',  ( -40.01497788969913927, 370.4323905765656377, -16.95518130045146421 ) ) ;
#15194 = DIRECTION ( 'NONE',  ( 0.000000000000000000, -1.000000000000000000, 0.000000000000000000 ) ) ;
#15195 = LINE ( 'NONE', #16815, #15131 ) ;
#15196 = CARTESIAN_POINT ( 'NONE',  ( -38.17536295476244135, 325.4323905683720000, 14.20200298773971781 ) ) ;
#15197 = PLANE ( 'NONE',  #8983 ) ;
#15198 = CARTESIAN_POINT ( 'NONE',  ( -45.43829269268871940, 475.0573905683720000, -3.332260488124726194 ) ) ;
#15199 = CARTESIAN_POINT ( 'NONE',  ( 154.7587007620219026, 620.7448905601785327, 10.81142786866622885 ) ) ;
#15200 = CARTESIAN_POINT ( 'NONE',  ( -10.20829729246297823, 302.8698905601784759, -7.653668647301794969 ) ) ;
#15201 = VECTOR ( 'NONE', #779, 1000.000000000000000 ) ;
#15202 = CARTESIAN_POINT ( 'NONE',  ( -16.84014894278199392, 391.6198905683720568, -11.84573899990672707 ) ) ;
#15203 = DIRECTION ( 'NONE',  ( -1.000000000000000000, -0.000000000000000000, -0.000000000000000000 ) ) ;
#15204 = CARTESIAN_POINT ( 'NONE',  ( -14.54375231895778953, 523.4948905601785327, -14.14213562373094746 ) ) ;
#15205 = CARTESIAN_POINT ( 'NONE',  ( -25.35362745456399125, 361.0573905683720000, -16.75240474999999307 ) ) ;
#15206 =( GEOMETRIC_REPRESENTATION_CONTEXT ( 3 ) GLOBAL_UNCERTAINTY_ASSIGNED_CONTEXT ( ( #7432 ) ) GLOBAL_UNIT_ASSIGNED_CONTEXT ( ( #16819, #386, #1571 ) ) REPRESENTATION_CONTEXT ( 'NONE', 'WORKASPACE' ) );
#15207 = ORIENTED_EDGE ( 'NONE', *, *, #867, .T. ) ;
#15208 = CARTESIAN_POINT ( 'NONE',  ( -40.53162694259545873, 532.6198905683720568, -11.84573899990672707 ) ) ;
#15209 = EDGE_LOOP ( 'NONE', ( #3038, #4236, #20591, #7279, #2666, #11351 ) ) ;
#15210 = CARTESIAN_POINT ( 'NONE',  ( -44.16309181155858710, 514.4948905683720568, 6.410867750099241924 ) ) ;
#15211 = EDGE_LOOP ( 'NONE', ( #10391, #21334, #15452, #10474, #20787, #16650, #9116 ) ) ;
#15212 = CARTESIAN_POINT ( 'NONE',  ( -36.33955658999052929, 530.1198905765655809, -18.47759065022572855 ) ) ;
#15213 = CARTESIAN_POINT ( 'NONE',  ( -42.88789093042844769, 492.9323905683720568, -9.489475012073736337 ) ) ;
#15214 = VERTEX_POINT ( 'NONE', #7924 ) ;
#15215 = CARTESIAN_POINT ( 'NONE',  ( -45.43829269268872650, 493.8698905683720568, 0.000000000000000000 ) ) ;
#15216 = DIRECTION ( 'NONE',  ( 0.000000000000000000, 0.000000000000000000, -1.000000000000000000 ) ) ;
#15217 = CARTESIAN_POINT ( 'NONE',  ( -28.68588794268872277, 419.4948905765656377, -19.99999999999999289 ) ) ;
#15218 = LINE ( 'NONE', #18649, #3411 ) ;
#15219 = DIRECTION ( 'NONE',  ( -1.000000000000000000, -0.000000000000000000, -0.000000000000000000 ) ) ;
#15220 = FACE_OUTER_BOUND ( 'NONE', #8958, .T. ) ;
#15221 = DIRECTION ( 'NONE',  ( 0.000000000000000000, 1.000000000000000000, -0.000000000000000000 ) ) ;
#15222 = PLANE ( 'NONE',  #10071 ) ;
#15223 = CARTESIAN_POINT ( 'NONE',  ( -48.68588794268881514, 492.3073905765656946, 3.978247347592954952 ) ) ;
#15224 = CARTESIAN_POINT ( 'NONE',  ( -35.09675569278793716, 293.4948905683720000, -15.47720386886985544 ) ) ;
#15225 = CARTESIAN_POINT ( 'NONE',  ( -48.68588794268875120, 527.5573905601784190, 3.978247347593114824 ) ) ;
#15226 = CARTESIAN_POINT ( 'NONE',  ( -42.88789093042844769, 454.4323905683720568, -9.489475012073736337 ) ) ;
#15227 = CARTESIAN_POINT ( 'NONE',  ( -28.68588794268871922, 414.4948905765656377, 19.99999999999999289 ) ) ;
#15228 = CARTESIAN_POINT ( 'NONE',  ( -40.53162694259542320, 266.6198905683720568, 11.84573899990672885 ) ) ;
#15229 = ORIENTED_EDGE ( 'NONE', *, *, #4546, .F. ) ;
#15230 = CARTESIAN_POINT ( 'NONE',  ( 148.8141120573112914, 400.5398297725603243, 0.000000000000000000 ) ) ;
#15231 = CARTESIAN_POINT ( 'NONE',  ( -13.20868407381887799, 500.9948905683721136, -6.410867750099233042 ) ) ;
#15232 = EDGE_CURVE ( 'NONE', #232, #8850, #1247, .T. ) ;
#15233 = VECTOR ( 'NONE', #19716, 1000.000000000000000 ) ;
#15234 = AXIS2_PLACEMENT_3D ( 'NONE', #19672, #8420, #1625 ) ;
#15235 = ORIENTED_EDGE ( 'NONE', *, *, #8471, .F. ) ;
#15236 = CARTESIAN_POINT ( 'NONE',  ( -19.19641293061498999, 458.8073905683720000, 14.20200298773971426 ) ) ;
#15237 = EDGE_CURVE ( 'NONE', #5798, #12056, #18209, .T. ) ;
#15238 = LINE ( 'NONE', #428, #17629 ) ;
#15239 = CARTESIAN_POINT ( 'NONE',  ( -16.84014894278197971, 260.1198905683720568, -11.84573899990672707 ) ) ;
#15240 = AXIS2_PLACEMENT_3D ( 'NONE', #19373, #8297, #4559 ) ;
#15241 = ORIENTED_EDGE ( 'NONE', *, *, #1256, .T. ) ;
#15242 = CARTESIAN_POINT ( 'NONE',  ( -28.68588794268870856, 334.4948905765656377, 19.99999999999999289 ) ) ;
#15243 = CARTESIAN_POINT ( 'NONE',  ( -22.27502019258946575, 268.4948905683720000, 15.47720386886985189 ) ) ;
#15244 = FACE_OUTER_BOUND ( 'NONE', #16010, .T. ) ;
#15245 = CARTESIAN_POINT ( 'NONE',  ( -32.01814843081343298, 243.1823905683720284, -16.75240474999999307 ) ) ;
#15246 = PRODUCT_DEFINITION_FORMATION_WITH_SPECIFIED_SOURCE ( 'ANY', '', #19431, .NOT_KNOWN. ) ;
#15247 = CARTESIAN_POINT ( 'NONE',  ( 51.50493485826542894, 160.1716627696692683, 61.61851857202071869 ) ) ;
#15248 = CARTESIAN_POINT ( 'NONE',  ( -28.68588794268874054, 573.2448905601785327, 0.000000000000000000 ) ) ;
#15249 = CARTESIAN_POINT ( 'NONE',  ( -13.20868407381884779, 259.4948905683720568, -6.410867750099233042 ) ) ;
#15250 = CARTESIAN_POINT ( 'NONE',  ( -28.68588794268871567, 362.8698905683720000, -16.75240474999999307 ) ) ;
#15251 = FACE_OUTER_BOUND ( 'NONE', #2782, .T. ) ;
#15252 = AXIS2_PLACEMENT_3D ( 'NONE', #13017, #14657, #4479 ) ;
#15253=STYLED_ITEM('',(#21442),#4901);
#15254 = APPLICATION_CONTEXT ( 'automotive_design' ) ;
#15255 = B_SPLINE_CURVE_WITH_KNOTS ( 'NONE', 3,
 ( #3270, #1541, #8112, #14745, #4882, #9845, #28, #13435, #1873, #11799, #18396, #10485, #6922, #3583, #11905, #10063, #7237, #7029, #464, #2181, #20027, #13651, #15170, #20236 ),
 .UNSPECIFIED., .F., .F.,
 ( 4, 2, 2, 2, 2, 2, 2, 2, 2, 2, 2, 4 ),
 ( 2.860979249076398407E-17, 0.002281674285428699801, 0.003422511428143036692, 0.004563348570857373582, 0.006845022856286023076, 0.007985859999000345655, 0.009126697141714665631, 0.01140837142714332640, 0.01369004571257198544, 0.01483088285528631235, 0.01597171999800063927, 0.01825339428342929657 ),
 .UNSPECIFIED. ) ;
#15256 = EDGE_CURVE ( 'NONE', #19850, #14887, #2334, .T. ) ;
#15257 = CARTESIAN_POINT ( 'NONE',  ( -28.68588794268872277, 411.3698905683720568, -16.75240474999999307 ) ) ;
#15258 = CARTESIAN_POINT ( 'NONE',  ( 5.074999999999999289, 0.000000000000000000, 0.000000000000000000 ) ) ;
#15259 = VECTOR ( 'NONE', #12629, 1000.000000000000000 ) ;
#15260 = CARTESIAN_POINT ( 'NONE',  ( -48.68588794268871567, 407.5573905601784759, 3.978247347593168115 ) ) ;
#15261 = ORIENTED_EDGE ( 'NONE', *, *, #648, .T. ) ;
#15262 = DIRECTION ( 'NONE',  ( -1.000000000000000000, -1.191790137725560488E-16, 0.000000000000000000 ) ) ;
#15263 = ORIENTED_EDGE ( 'NONE', *, *, #4201, .F. ) ;
#15264 = VERTEX_POINT ( 'NONE', #14452 ) ;
#15265 = CARTESIAN_POINT ( 'NONE',  ( -16.84014894278200458, 519.1198905683720568, 11.84573899990672530 ) ) ;
#15266 = CARTESIAN_POINT ( 'NONE',  ( -21.03221929538690205, 280.3698905601784759, 18.47759065022572500 ) ) ;
#15267 = CARTESIAN_POINT ( 'NONE',  ( -48.68588794268853803, 321.6823905765655809, -3.978247347593583783 ) ) ;
#15268 = VERTEX_POINT ( 'NONE', #15963 ) ;
#15269 = CARTESIAN_POINT ( 'NONE',  ( -28.68588794268871212, 332.8698905683720000, -16.75240474999999307 ) ) ;
#15270 = ORIENTED_EDGE ( 'NONE', *, *, #3235, .T. ) ;
#15271 = CARTESIAN_POINT ( 'NONE',  ( -44.16309181155856578, 364.4948905683720568, 6.410867750099241924 ) ) ;
#15272 = CARTESIAN_POINT ( 'NONE',  ( -11.93348319268872260, 368.5573905683719431, 3.332260488124728859 ) ) ;
#15273 = EDGE_CURVE ( 'NONE', #9516, #15951, #4051, .T. ) ;
#15274 = CARTESIAN_POINT ( 'NONE',  ( -17.35679799567829207, 298.5573905765656377, -16.95518130045146421 ) ) ;
#15275 = CARTESIAN_POINT ( 'NONE',  ( 5.074999999999999289, 6.500000000000000888, 0.000000000000000000 ) ) ;
#15276 = CARTESIAN_POINT ( 'NONE',  ( -38.17536295476244135, 262.3073905683720568, -14.20200298773971426 ) ) ;
#15277 = DIRECTION ( 'NONE',  ( 0.6352526299242177155, 0.000000000000000000, 0.7723044064191041391 ) ) ;
#15278 =( BOUNDED_CURVE ( )  B_SPLINE_CURVE ( 2, ( #966, #12633, #19004, #17599, #1072, #2790, #6023, #14266, #9155, #20956, #2575, #21060, #19224, #7642, #12525, #10990, #7850 ),
 .UNSPECIFIED., .F., .T. ) 
 B_SPLINE_CURVE_WITH_KNOTS ( ( 3, 2, 2, 2, 2, 2, 2, 2, 3 ),
 ( 0.7656250000000001110, 0.7675781250000001110, 0.7695312500000001110, 0.7714843750000001110, 0.7734375000000001110, 0.7753906250000001110, 0.7773437500000001110, 0.7792968750000001110, 0.7812500000000001110 ),
 .UNSPECIFIED. ) 
 CURVE ( )  GEOMETRIC_REPRESENTATION_ITEM ( )  RATIONAL_B_SPLINE_CURVE ( ( 0.9999999999999988898, 0.9807852804032315408, 1.000000000000000000, 0.9807852804032304306, 1.000000000000000000, 0.9807852804032304306, 1.000000000000000000, 0.9807852804032304306, 1.000000000000000000, 0.9807852804032304306, 1.000000000000000000, 0.9807852804032304306, 1.000000000000000000, 0.9807852804032304306, 1.000000000000000000, 0.9807852804032293204, 1.000000000000001110 ) ) 
 REPRESENTATION_ITEM ( '' )  );
#15279 = CARTESIAN_POINT ( 'NONE',  ( -11.93348319268872793, 420.3698905683720568, -2.051577885510841163E-15 ) ) ;
#15280 = FACE_BOUND ( 'NONE', #5348, .T. ) ;
#15281 = CARTESIAN_POINT ( 'NONE',  ( -28.68588794268872633, 449.4948905765655809, -19.99999999999999289 ) ) ;
#15282 = CARTESIAN_POINT ( 'NONE',  ( 6.416697501590670427, 217.7548513357008630, 49.99999999999999289 ) ) ;
#15283 = ADVANCED_FACE ( 'NONE', ( #19512, #17678, #13135 ), #13355, .F. ) ;
#15284 = CARTESIAN_POINT ( 'NONE',  ( -11.93348319268871904, 330.6823905683721136, -3.332260488124732856 ) ) ;
#15285 = CARTESIAN_POINT ( 'NONE',  ( -16.84014894278200458, 470.1198905683720568, -11.84573899990672707 ) ) ;
#15286 = ORIENTED_EDGE ( 'NONE', *, *, #12612, .T. ) ;
#15287 = CARTESIAN_POINT ( 'NONE',  ( -42.82802356641967378, 458.4948905601784759, 14.14213562373094923 ) ) ;
#15288 = CARTESIAN_POINT ( 'NONE',  ( -40.53162694259543031, 282.6198905683720000, -11.84573899990672707 ) ) ;
#15289 = CARTESIAN_POINT ( 'NONE',  ( -17.35679799567828852, 345.4323905765656377, 16.95518130045146421 ) ) ;
#15290 = EDGE_LOOP ( 'NONE', ( #12884, #17069, #3773 ) ) ;
#15291 = CARTESIAN_POINT ( 'NONE',  ( 75.04415151326509203, 162.3117964647028373, -60.96179693900064933 ) ) ;
#15292 = CARTESIAN_POINT ( 'NONE',  ( -11.73070664223724968, 343.1823905601785327, -11.32908994701042715 ) ) ;
#15293 = CARTESIAN_POINT ( 'NONE',  ( -38.17536295476244845, 302.3073905683720568, -14.20200298773971426 ) ) ;
#15294 = CARTESIAN_POINT ( 'NONE',  ( -25.35362745456398414, 388.1823905683720568, 16.75240474999998952 ) ) ;
#15295 = CARTESIAN_POINT ( 'NONE',  ( -8.685887942688625074, 292.5573905601784190, -3.978247347592952732 ) ) ;
#15296 = DIRECTION ( 'NONE',  ( -1.000000000000000000, 0.000000000000000000, 0.000000000000000000 ) ) ;
#15297 = CARTESIAN_POINT ( 'NONE',  ( -25.35362745456398770, 426.6823905683720568, 16.75240474999998952 ) ) ;
#15298 = CARTESIAN_POINT ( 'NONE',  ( -28.68588794268869790, 257.8698905683720000, 16.75240474999999307 ) ) ;
#15299 = CARTESIAN_POINT ( 'NONE',  ( -25.35362745456399836, 431.0573905683720000, -16.75240474999999307 ) ) ;
#15300 = SHAPE_DEFINITION_REPRESENTATION ( #6125, #4206 ) ;
#15301 = CARTESIAN_POINT ( 'NONE',  ( -8.685887942688722774, 367.3073905765656946, -3.978247347593165895 ) ) ;
#15302 = CYLINDRICAL_SURFACE ( 'NONE', #12409, 11.54039041455135184 ) ;
#15303 = CARTESIAN_POINT ( 'NONE',  ( -14.48388495494899608, 329.8073905683720568, -9.489475012073734561 ) ) ;
#15304 = VECTOR ( 'NONE', #970, 1000.000000000000000 ) ;
#15305 = CARTESIAN_POINT ( 'NONE',  ( -45.43829269268871940, 485.6823905683721136, 3.332260488124734632 ) ) ;
#15306 = B_SPLINE_CURVE_WITH_KNOTS ( 'NONE', 3,
 ( #9584, #9265, #15883, #1071, #12632, #7641 ),
 .UNSPECIFIED., .F., .F.,
 ( 4, 2, 4 ),
 ( 2.380733003144577723E-07, 0.001898835937927388726, 0.003797433802554463222 ),
 .UNSPECIFIED. ) ;
#15307 = CARTESIAN_POINT ( 'NONE',  ( 29.72350413846044859, 280.4463447002762564, -20.00000000000000355 ) ) ;
#15308 = DIRECTION ( 'NONE',  ( -1.000000000000000000, -0.000000000000000000, -0.000000000000000000 ) ) ;
#15309 = CARTESIAN_POINT ( 'NONE',  ( -14.54375231895776288, 303.4948905601784759, -14.14213562373094746 ) ) ;
#15310 = CARTESIAN_POINT ( 'NONE',  ( -38.17536295476246266, 393.8073905683720000, -14.20200298773971426 ) ) ;
#15311 = CARTESIAN_POINT ( 'NONE',  ( -29.29923972067796356, 47.64464476306663698, -121.5194033971115601 ) ) ;
#15312 = ADVANCED_FACE ( 'NONE', ( #18204 ), #1676, .T. ) ;
#15313 = CIRCLE ( 'NONE', #10436, 15.00000000000000355 ) ;
#15314 = CARTESIAN_POINT ( 'NONE',  ( -21.03221929538694468, 534.1198905601785327, -18.47759065022572855 ) ) ;
#15315 = CARTESIAN_POINT ( 'NONE',  ( -16.84014894278199037, 350.1198905683720568, -11.84573899990672707 ) ) ;
#15316 = ADVANCED_FACE ( 'NONE', ( #1899 ), #4907, .F. ) ;
#15317 = ORIENTED_EDGE ( 'NONE', *, *, #9407, .F. ) ;
#15318 = CARTESIAN_POINT ( 'NONE',  ( -25.35362745456401257, 531.0573905683720568, -16.75240474999999307 ) ) ;
#15319 = ORIENTED_EDGE ( 'NONE', *, *, #1933, .F. ) ;
#15320 = CARTESIAN_POINT ( 'NONE',  ( -45.43829269268872650, 513.5573905683719431, -3.332260488124726194 ) ) ;
#15321 = ORIENTED_EDGE ( 'NONE', *, *, #16505, .F. ) ;
#15322 = CARTESIAN_POINT ( 'NONE',  ( -18.81370552131602736, 585.7448905601785327, 6.112943483001358480 ) ) ;
#15323 = CARTESIAN_POINT ( 'NONE',  ( -32.01814843081346140, 481.6823905683720568, -16.75240474999999307 ) ) ;
#15324 = VERTEX_POINT ( 'NONE', #59 ) ;
#15325 = CARTESIAN_POINT ( 'NONE',  ( -42.88789093042844769, 482.9323905683720000, -9.489475012073734561 ) ) ;
#15326 = CARTESIAN_POINT ( 'NONE',  ( -15.94757079417145462, 47.22349452202089282, -47.93784354121613234 ) ) ;
#15327 = EDGE_CURVE ( 'NONE', #13421, #9261, #5590, .T. ) ;
#15328 = AXIS2_PLACEMENT_3D ( 'NONE', #13559, #18300, #3697 ) ;
#15329 = CARTESIAN_POINT ( 'NONE',  ( -42.82802356641966668, 430.7448905765656377, -14.14213562373094746 ) ) ;
#15330 = CARTESIAN_POINT ( 'NONE',  ( 125.7989814974898337, 160.1716627696691830, 40.00000000000000000 ) ) ;
#15331 = DIRECTION ( 'NONE',  ( 0.000000000000000000, -1.000000000000000000, 0.000000000000000000 ) ) ;
#15332 = CARTESIAN_POINT ( 'NONE',  ( -21.03221929538693402, 438.8698905765656377, -18.47759065022572855 ) ) ;
#15333 = CARTESIAN_POINT ( 'NONE',  ( 91.21585410611801592, 56.85652257517428865, 94.99999999999994316 ) ) ;
#15334 = VECTOR ( 'NONE', #8657, 1000.000000000000000 ) ;
#15335 = EDGE_CURVE ( 'NONE', #4920, #6399, #11613, .T. ) ;
#15336 = DIRECTION ( 'NONE',  ( -1.000000000000000000, 0.000000000000000000, 0.000000000000000000 ) ) ;
#15337 = CARTESIAN_POINT ( 'NONE',  ( 2.416697501590669095, 217.7548513357008630, 60.00000000000000000 ) ) ;
#15338 = CARTESIAN_POINT ( 'NONE',  ( -22.27502019258947996, 302.2448905683720000, -15.47720386886985544 ) ) ;
#15339 = DIRECTION ( 'NONE',  ( -0.000000000000000000, 1.000000000000000000, -0.000000000000000000 ) ) ;
#15340 = CARTESIAN_POINT ( 'NONE',  ( -38.17536295476245556, 446.9323905683720000, 14.20200298773971781 ) ) ;
#15341 = CARTESIAN_POINT ( 'NONE',  ( -24.70764059509556176, 399.1823905765656377, -19.99999999999999289 ) ) ;
#15342 = CARTESIAN_POINT ( 'NONE',  ( -45.43829269268870519, 275.3698905683720000, 0.000000000000000000 ) ) ;
#15343 = ADVANCED_FACE ( 'NONE', ( #17990 ), #8135, .T. ) ;
#15344 = AXIS2_PLACEMENT_3D ( 'NONE', #20918, #12375, #4147 ) ;
#15345 = ORIENTED_EDGE ( 'NONE', *, *, #14790, .F. ) ;
#15346 = CARTESIAN_POINT ( 'NONE',  ( -24.70764059509557953, 534.4323905601784190, -19.99999999999999289 ) ) ;
#15347 = CARTESIAN_POINT ( 'NONE',  ( -45.43829269268872650, 485.3698905683720568, 0.000000000000000000 ) ) ;
#15348 = AXIS2_PLACEMENT_3D ( 'NONE', #3893, #20661, #20449 ) ;
#15349 = ORIENTED_EDGE ( 'NONE', *, *, #4926, .F. ) ;
#15350 = CARTESIAN_POINT ( 'NONE',  ( -35.09675569278796559, 457.2448905683720568, 15.47720386886985366 ) ) ;
#15351 = CARTESIAN_POINT ( 'NONE',  ( -32.66413529028187668, 409.8073905765656377, -19.99999999999999289 ) ) ;
#15352 = CARTESIAN_POINT ( 'NONE',  ( -19.19641293061496867, 257.3073905683720568, 14.20200298773971426 ) ) ;
#15353 = EDGE_LOOP ( 'NONE', ( #21126, #5616 ) ) ;
#15354 = CARTESIAN_POINT ( 'NONE',  ( -47.16347859291444422, 332.6198905765656377, 7.653668647301805628 ) ) ;
#15355 = CARTESIAN_POINT ( 'NONE',  ( -8.685887942688736985, 477.3073905765656377, -3.978247347593165895 ) ) ;
#15356 = CARTESIAN_POINT ( 'NONE',  ( -8.685887942688726326, 392.2448905601784759, -2.449293598294705724E-15 ) ) ;
#15357 = CARTESIAN_POINT ( 'NONE',  ( -44.16309181155855157, 235.9948905683720284, 6.410867750099241924 ) ) ;
#15358 = CARTESIAN_POINT ( 'NONE',  ( -36.33955658999051508, 420.1198905765656377, -18.47759065022572855 ) ) ;
#15359 = CARTESIAN_POINT ( 'NONE',  ( -45.64106924314017277, 238.1823905601785043, 11.32908994701042715 ) ) ;
#15360 = CARTESIAN_POINT ( 'NONE',  ( -35.09675569278793006, 241.9948905683720284, -15.47720386886985544 ) ) ;
#15361 = VECTOR ( 'NONE', #5529, 1000.000000000000114 ) ;
#15362 = CARTESIAN_POINT ( 'NONE',  ( -40.53162694259543741, 366.6198905683720000, 11.84573899990672885 ) ) ;
#15363 = CARTESIAN_POINT ( 'NONE',  ( -49.57497958038185715, 160.1716627696692683, -50.00000000000000000 ) ) ;
#15364 = ADVANCED_FACE ( 'NONE', ( #9869 ), #6844, .F. ) ;
#15365 = CARTESIAN_POINT ( 'NONE',  ( -14.48388495494900496, 409.8073905683720568, -9.489475012073736337 ) ) ;
#15366 = CARTESIAN_POINT ( 'NONE',  ( -36.33955658999050797, 340.1198905765655809, -18.47759065022572855 ) ) ;
#15367 = CARTESIAN_POINT ( 'NONE',  ( -45.64106924314019409, 406.3073905601784759, -11.32908994701042715 ) ) ;
#15368 = ORIENTED_EDGE ( 'NONE', *, *, #12350, .T. ) ;
#15369 = CARTESIAN_POINT ( 'NONE',  ( -42.82802356641965957, 350.7448905765655809, -14.14213562373094746 ) ) ;
#15370 = ORIENTED_EDGE ( 'NONE', *, *, #3816, .T. ) ;
#15371 = EDGE_LOOP ( 'NONE', ( #5075, #5823, #18889, #20670 ) ) ;
#15372 = CARTESIAN_POINT ( 'NONE',  ( -40.53162694259545873, 524.1198905683720568, -11.84573899990672707 ) ) ;
#15373 = CARTESIAN_POINT ( 'NONE',  ( -14.54375231895775578, 280.9948905601785327, 14.14213562373094568 ) ) ;
#15374 = DIRECTION ( 'NONE',  ( -1.000000000000000000, 0.000000000000000000, -0.000000000000000000 ) ) ;
#15375 = CARTESIAN_POINT ( 'NONE',  ( -13.20868407381885490, 329.7448905683720568, 6.410867750099229490 ) ) ;
#15376 = EDGE_LOOP ( 'NONE', ( #8959, #7116, #17948, #12939 ) ) ;
#15377 = CARTESIAN_POINT ( 'NONE',  ( -28.68588794268871212, 341.3698905683720000, -16.75240474999999307 ) ) ;
#15378 = CARTESIAN_POINT ( 'NONE',  ( -19.19641293061497933, 357.3073905683720000, 14.20200298773971426 ) ) ;
#15379 = EDGE_CURVE ( 'NONE', #573, #502, #13057, .T. ) ;
#15380 = CARTESIAN_POINT ( 'NONE',  ( -28.68588794268870146, 274.4948905765656377, 19.99999999999999289 ) ) ;
#15381 = CARTESIAN_POINT ( 'NONE',  ( -162.2727221670389781, 30.52886280891152282, -20.57735571454641033 ) ) ;
#15382 = CARTESIAN_POINT ( 'NONE',  ( -25.35362745456396993, 266.6823905683720568, 16.75240474999998952 ) ) ;
#15383 = CARTESIAN_POINT ( 'NONE',  ( -43.31864445205426506, 201.3798797254112856, 3.307266650052995693 ) ) ;
#15384 = CARTESIAN_POINT ( 'NONE',  ( -32.01814843081345430, 417.5573905683720568, 16.75240474999999307 ) ) ;
#15385 = CARTESIAN_POINT ( 'NONE',  ( 28.16023193154655502, 323.8848358243226357, 40.00000000000000000 ) ) ;
#15386 = DIRECTION ( 'NONE',  ( 0.000000000000000000, 0.000000000000000000, 1.000000000000000000 ) ) ;
#15387 = CARTESIAN_POINT ( 'NONE',  ( -44.16309181155855867, 325.9948905683720000, 6.410867750099241924 ) ) ;
#15388 = CARTESIAN_POINT ( 'NONE',  ( -28.68588794268872633, 466.3698905683720000, 16.75240474999999307 ) ) ;
#15389 = ORIENTED_EDGE ( 'NONE', *, *, #6426, .F. ) ;
#15390 = CARTESIAN_POINT ( 'NONE',  ( -47.16347859291445843, 476.6198905601785327, -7.653668647301793193 ) ) ;
#15391 = CARTESIAN_POINT ( 'NONE',  ( -25.35362745456397349, 286.6823905683720568, 16.75240474999998952 ) ) ;
#15392 = EDGE_CURVE ( 'NONE', #2119, #13766, #15195, .T. ) ;
#15393 = ORIENTED_EDGE ( 'NONE', *, *, #12854, .T. ) ;
#15394 = ORIENTED_EDGE ( 'NONE', *, *, #16052, .T. ) ;
#15395 = CARTESIAN_POINT ( 'NONE',  ( 78.68120802659203150, 149.7457237375499517, -66.14548919766382085 ) ) ;
#15396 = CARTESIAN_POINT ( 'NONE',  ( -25.35362745456397349, 296.6823905683720000, 16.75240474999998952 ) ) ;
#15397 = CARTESIAN_POINT ( 'NONE',  ( -44.16309181155856578, 375.9948905683720568, 6.410867750099241924 ) ) ;
#15398 = DIRECTION ( 'NONE',  ( 0.02283316540262222277, -0.9997392892938120612, -0.000000000000000000 ) ) ;
#15399 = CARTESIAN_POINT ( 'NONE',  ( -10.20829729246300666, 526.3698905765656946, 7.653668647301790529 ) ) ;
#15400 = CARTESIAN_POINT ( 'NONE',  ( -14.48388495494900496, 399.8073905683720568, -9.489475012073736337 ) ) ;
#15401 = CARTESIAN_POINT ( 'NONE',  ( -44.16309181155855157, 255.9948905683720568, 6.410867750099241924 ) ) ;
#15402 = CARTESIAN_POINT ( 'NONE',  ( -35.09675569278795848, 435.7448905683720000, 15.47720386886985366 ) ) ;
#15403 = CONTEXT_DEPENDENT_SHAPE_REPRESENTATION ( #15540, #4748 ) ;
#15404 =( BOUNDED_CURVE ( )  B_SPLINE_CURVE ( 2, ( #11906, #7346, #5409, #13549, #13865, #7238, #15703, #13979, #15281, #12013, #2182, #3999, #2287, #2500, #465, #5728, #17109 ),
 .UNSPECIFIED., .F., .T. ) 
 B_SPLINE_CURVE_WITH_KNOTS ( ( 3, 2, 2, 2, 2, 2, 2, 2, 3 ),
 ( 0.2500000000000002220, 0.2519531250000002220, 0.2539062500000002220, 0.2558593750000002220, 0.2578125000000002220, 0.2597656250000002220, 0.2617187500000002220, 0.2636718750000002220, 0.2656250000000002220 ),
 .UNSPECIFIED. ) 
 CURVE ( )  GEOMETRIC_REPRESENTATION_ITEM ( )  RATIONAL_B_SPLINE_CURVE ( ( 0.9999999999999977796, 0.9807852804032326510, 1.000000000000000000, 0.9807852804032304306, 1.000000000000000000, 0.9807852804032304306, 1.000000000000000000, 0.9807852804032304306, 1.000000000000000000, 0.9807852804032304306, 1.000000000000000000, 0.9807852804032304306, 1.000000000000000000, 0.9807852804032304306, 1.000000000000000000, 0.9807852804032282101, 1.000000000000002220 ) ) 
 REPRESENTATION_ITEM ( '' )  );
#15405 = ADVANCED_FACE ( 'NONE', ( #18421 ), #8572, .T. ) ;
#15406 = CARTESIAN_POINT ( 'NONE',  ( -45.64106924314018698, 362.9323905765656377, 11.32908994701042715 ) ) ;
#15407 = EDGE_CURVE ( 'NONE', #9092, #8857, #2004, .T. ) ;
#15408 = CARTESIAN_POINT ( 'NONE',  ( -40.01497788969913216, 275.6823905601784759, -16.95518130045146421 ) ) ;
#15409 = CARTESIAN_POINT ( 'NONE',  ( -35.09675569278794427, 325.7448905683720000, 15.47720386886985366 ) ) ;
#15410 = CARTESIAN_POINT ( 'NONE',  ( -40.01497788969913927, 433.5573905765656946, 16.95518130045146776 ) ) ;
#15411 = CARTESIAN_POINT ( 'NONE',  ( 81.24038404635966515, 30.52886280891152282, 94.99999999999994316 ) ) ;
#15412 = DIRECTION ( 'NONE',  ( -0.4989387216749512355, -0.8666372666885295839, -0.000000000000000000 ) ) ;
#15413 = CARTESIAN_POINT ( 'NONE',  ( -28.68588794268871567, 387.8698905683720000, 16.75240474999999307 ) ) ;
#15414 = DIRECTION ( 'NONE',  ( 3.836511174089486173E-16, -0.000000000000000000, 1.000000000000000000 ) ) ;
#15415 = CARTESIAN_POINT ( 'NONE',  ( -32.66413529028189799, 519.4323905601784190, 19.99999999999999289 ) ) ;
#15416 = CARTESIAN_POINT ( 'NONE',  ( -35.09675569278795138, 345.7448905683720568, 15.47720386886985366 ) ) ;
#15417 = VERTEX_POINT ( 'NONE', #4613 ) ;
#15418 = CARTESIAN_POINT ( 'NONE',  ( -40.53162694259545873, 505.1198905683720568, 11.84573899990672885 ) ) ;
#15419 = VERTEX_POINT ( 'NONE', #20950 ) ;
#15420 = CARTESIAN_POINT ( 'NONE',  ( 51.50493485826542184, 170.1716627696692683, 57.52045949366692668 ) ) ;
#15421 = CARTESIAN_POINT ( 'NONE',  ( -40.01497788969913216, 315.6823905601785327, -16.95518130045146421 ) ) ;
#15422 = DIRECTION ( 'NONE',  ( -0.000000000000000000, -0.000000000000000000, -1.000000000000000000 ) ) ;
#15423 =( LENGTH_UNIT ( ) NAMED_UNIT ( * ) SI_UNIT ( .MILLI., .METRE. ) );
#15424 = CARTESIAN_POINT ( 'NONE',  ( -28.68588794268872277, 456.3698905683720000, 16.75240474999999307 ) ) ;
#15425 = ORIENTED_EDGE ( 'NONE', *, *, #10583, .T. ) ;
#15426 = CARTESIAN_POINT ( 'NONE',  ( -25.35362745456400901, 491.0573905683720568, -16.75240474999999307 ) ) ;
#15427 = CARTESIAN_POINT ( 'NONE',  ( 60.03793209889851568, 10.52886280891152104, -152.3753892284480003 ) ) ;
#15428 = CARTESIAN_POINT ( 'NONE',  ( -36.33955658999051508, 430.1198905765656377, -18.47759065022572855 ) ) ;
#15429 = CARTESIAN_POINT ( 'NONE',  ( -48.68588794268872277, 471.9948905765656377, 0.000000000000000000 ) ) ;
#15430 = DIRECTION ( 'NONE',  ( 1.000000000000000000, 0.000000000000000000, 0.000000000000000000 ) ) ;
#15431 = CARTESIAN_POINT ( 'NONE',  ( 3.458603197740078627, 303.6587712403113528, 33.59072564020503648 ) ) ;
#15432 = CARTESIAN_POINT ( 'NONE',  ( -47.16347859291445843, 482.6198905765656377, 7.653668647301805628 ) ) ;
#15433 = CARTESIAN_POINT ( 'NONE',  ( -28.68588794268873698, 548.2448905601784190, 0.000000000000000000 ) ) ;
#15434 = CARTESIAN_POINT ( 'NONE',  ( -28.68588794268875120, 610.7448905601785327, 0.000000000000000000 ) ) ;
#15435 = DIRECTION ( 'NONE',  ( -8.901024030850960568E-17, 0.000000000000000000, 1.000000000000000000 ) ) ;
#15436 = CARTESIAN_POINT ( 'NONE',  ( -25.35362745456398059, 282.5573905683720568, -16.75240474999999307 ) ) ;
#15437 = CARTESIAN_POINT ( 'NONE',  ( -40.01497788969911795, 248.8073905601784759, 16.95518130045146776 ) ) ;
#15438 = CARTESIAN_POINT ( 'NONE',  ( -14.54375231895777176, 405.7448905765656377, 14.14213562373094568 ) ) ;
#15439 = CARTESIAN_POINT ( 'NONE',  ( -19.19641293061499354, 451.9323905683720568, -14.20200298773971603 ) ) ;
#15440 = CARTESIAN_POINT ( 'NONE',  ( 30.42502041961814996, 170.1716627696692683, 20.00000000000000355 ) ) ;
#15441 = CARTESIAN_POINT ( 'NONE',  ( -35.09675569278793006, 263.4948905683720000, -15.47720386886985544 ) ) ;
#15442 = EDGE_CURVE ( 'NONE', #17480, #11300, #13395, .T. ) ;
#15443 = EDGE_LOOP ( 'NONE', ( #19240, #17532, #20653, #17144 ) ) ;
#15444 = CARTESIAN_POINT ( 'NONE',  ( -32.66413529028189089, 535.0573905601784190, -19.99999999999999289 ) ) ;
#15445 = CARTESIAN_POINT ( 'NONE',  ( -42.88789093042844769, 476.3073905683719431, 9.489475012073734561 ) ) ;
#15446 = EDGE_CURVE ( 'NONE', #21369, #1587, #12232, .T. ) ;
#15447 = EDGE_CURVE ( 'NONE', #18701, #19677, #9717, .T. ) ;
#15448 = AXIS2_PLACEMENT_3D ( 'NONE', #12263, #10412, #7061 ) ;
#15449 = ORIENTED_EDGE ( 'NONE', *, *, #13259, .T. ) ;
#15450 = DIRECTION ( 'NONE',  ( 0.000000000000000000, 0.000000000000000000, 1.000000000000000000 ) ) ;
#15451 = CARTESIAN_POINT ( 'NONE',  ( -45.43829269268869808, 263.8698905683720000, 0.000000000000000000 ) ) ;
#15452 = ORIENTED_EDGE ( 'NONE', *, *, #14669, .F. ) ;
#15453 = AXIS2_PLACEMENT_3D ( 'NONE', #16607, #8364, #14987 ) ;
#15454 = CARTESIAN_POINT ( 'NONE',  ( -11.73070664223726212, 486.0573905765656946, 11.32908994701042005 ) ) ;
#15455 = CARTESIAN_POINT ( 'NONE',  ( -42.82802356641965957, 388.4948905601784759, 14.14213562373094923 ) ) ;
#15456 = CARTESIAN_POINT ( 'NONE',  ( -32.89526592549250950, 223.9102039777117170, -17.42271427295905184 ) ) ;
#15457 = CARTESIAN_POINT ( 'NONE',  ( -14.48388495494898365, 239.4323905683720000, 9.489475012073731008 ) ) ;
#15458 = EDGE_CURVE ( 'NONE', #5025, #11304, #7981, .T. ) ;
#15459 = CARTESIAN_POINT ( 'NONE',  ( -22.27502019258950483, 522.2448905683720568, -15.47720386886985544 ) ) ;
#15460 = CARTESIAN_POINT ( 'NONE',  ( 0.06682554136337878758, 6.264794173742276762, 2.149058192116893640 ) ) ;
#15461 = CARTESIAN_POINT ( 'NONE',  ( -13.20868407381884779, 249.4948905683720284, -6.410867750099233042 ) ) ;
#15462 = CARTESIAN_POINT ( 'NONE',  ( -11.93348319268871904, 340.3698905683720000, -2.051577885510841163E-15 ) ) ;
#15463 = AXIS2_PLACEMENT_3D ( 'NONE', #9344, #6203, #7822 ) ;
#15464 = CARTESIAN_POINT ( 'NONE',  ( 91.21585410611801592, 31.85652257517428865, -85.46735025547123143 ) ) ;
#15465 = AXIS2_PLACEMENT_3D ( 'NONE', #11366, #1764, #1653 ) ;
#15466 = CARTESIAN_POINT ( 'NONE',  ( -45.43829269268871229, 404.1823905683720568, 3.332260488124734632 ) ) ;
#15467 = LINE ( 'NONE', #2371, #13274 ) ;
#15468 = CARTESIAN_POINT ( 'NONE',  ( -8.685887942688726326, 412.5573905601785327, -3.978247347593165895 ) ) ;
#15469 = ORIENTED_EDGE ( 'NONE', *, *, #18476, .F. ) ;
#15470 = PLANE ( 'NONE',  #18063 ) ;
#15471 = EDGE_LOOP ( 'NONE', ( #2292, #4069, #20620, #7095 ) ) ;
#15472 = ORIENTED_EDGE ( 'NONE', *, *, #774, .T. ) ;
#15473 = CARTESIAN_POINT ( 'NONE',  ( -19.19641293061500065, 511.9323905683721136, -14.20200298773971603 ) ) ;
#15474 = CARTESIAN_POINT ( 'NONE',  ( -32.66413529028186957, 285.0573905601784759, -19.99999999999999289 ) ) ;
#15475 = CARTESIAN_POINT ( 'NONE',  ( -24.70764059509555466, 319.1823905765656377, -19.99999999999999289 ) ) ;
#15476 = EDGE_LOOP ( 'NONE', ( #5086, #16801, #13148, #1266, #7221 ) ) ;
#15477 = CARTESIAN_POINT ( 'NONE',  ( -45.43829269268870519, 325.3698905683720000, 0.000000000000000000 ) ) ;
#15478 = EDGE_LOOP ( 'NONE', ( #7911, #19210, #3146 ) ) ;
#15479 = CARTESIAN_POINT ( 'NONE',  ( -45.43829269268870519, 343.5573905683720000, -3.332260488124726194 ) ) ;
#15480 = CARTESIAN_POINT ( 'NONE',  ( -16.84014894278198682, 367.6198905683720000, 11.84573899990672530 ) ) ;
#15481 = CARTESIAN_POINT ( 'NONE',  ( -42.82802356641965247, 290.7448905765655809, -14.14213562373094746 ) ) ;
#15482 = DIRECTION ( 'NONE',  ( -1.191790137725560488E-16, 1.000000000000000000, -0.000000000000000000 ) ) ;
#15483 = CARTESIAN_POINT ( 'NONE',  ( -45.43829269268869808, 244.1823905683720568, 3.332260488124734632 ) ) ;
#15484 = DIRECTION ( 'NONE',  ( 0.000000000000000000, 0.000000000000000000, 1.000000000000000000 ) ) ;
#15485 = CARTESIAN_POINT ( 'NONE',  ( -32.01814843081345430, 413.1823905683719431, -16.75240474999999307 ) ) ;
#15486 = CARTESIAN_POINT ( 'NONE',  ( -42.82802356641965957, 335.9948905601784759, -14.14213562373094746 ) ) ;
#15487 = CARTESIAN_POINT ( 'NONE',  ( 0.000000000000000000, 7.505553499465139389, 0.000000000000000000 ) ) ;
#15488 = FACE_OUTER_BOUND ( 'NONE', #2164, .T. ) ;
#15489 = CARTESIAN_POINT ( 'NONE',  ( -25.35362745456398770, 322.5573905683720000, -16.75240474999999307 ) ) ;
#15490 = CARTESIAN_POINT ( 'NONE',  ( -35.09675569278796559, 455.7448905683720568, 15.47720386886985366 ) ) ;
#15491 = ORIENTED_EDGE ( 'NONE', *, *, #9827, .T. ) ;
#15492 = CARTESIAN_POINT ( 'NONE',  ( -11.73070664223725856, 471.3073905601784759, 11.32908994701042005 ) ) ;
#15493 = CARTESIAN_POINT ( 'NONE',  ( -11.93348319268871371, 289.1823905683720000, -3.332260488124732856 ) ) ;
#15494 = EDGE_CURVE ( 'NONE', #13185, #7305, #4847, .T. ) ;
#15495 = ORIENTED_EDGE ( 'NONE', *, *, #6915, .T. ) ;
#15496 = CARTESIAN_POINT ( 'NONE',  ( -28.68588794268872633, 442.8698905683720568, -16.75240474999999307 ) ) ;
#15497 = VERTEX_POINT ( 'NONE', #13082 ) ;
#15498 = CARTESIAN_POINT ( 'NONE',  ( -48.68588794268872988, 511.9948905765656377, 0.000000000000000000 ) ) ;
#15499 = CARTESIAN_POINT ( 'NONE',  ( -45.64106924314018698, 336.3073905601784759, -11.32908994701042715 ) ) ;
#15500 = CARTESIAN_POINT ( 'NONE',  ( -13.20868407381885135, 298.2448905683720000, 6.410867750099229490 ) ) ;
#15501 = CARTESIAN_POINT ( 'NONE',  ( -45.43829269268871229, 385.3698905683720568, 0.000000000000000000 ) ) ;
#15502 = CARTESIAN_POINT ( 'NONE',  ( -32.66413529028185536, 229.4323905601785043, 19.99999999999999289 ) ) ;
#15503 = EDGE_CURVE ( 'NONE', #20007, #19138, #19668, .T. ) ;
#15504 = CARTESIAN_POINT ( 'NONE',  ( -10.20829729246300488, 517.6198905765656946, -7.653668647301794969 ) ) ;
#15505 = CARTESIAN_POINT ( 'NONE',  ( -11.93348319268872615, 398.8698905683720000, -2.051577885510841163E-15 ) ) ;
#15506 = CARTESIAN_POINT ( 'NONE',  ( -38.17536295476243424, 246.9323905683720284, 14.20200298773971781 ) ) ;
#15507 = CARTESIAN_POINT ( 'NONE',  ( -32.01814843081344719, 431.6823905683720000, -16.75240474999999307 ) ) ;
#15508 = ITEM_DEFINED_TRANSFORMATION ( 'NONE', 'NONE', #13515,  #12794 ) ;
#15509 = AXIS2_PLACEMENT_3D ( 'NONE', #9777, #7836, #19737 ) ;
#15510 = CARTESIAN_POINT ( 'NONE',  ( -17.35679799567829207, 345.4323905765656377, 16.95518130045146421 ) ) ;
#15511 = DIRECTION ( 'NONE',  ( 1.000000000000000000, 0.000000000000000000, 0.000000000000000000 ) ) ;
#15512 = CARTESIAN_POINT ( 'NONE',  ( -35.09675569278795138, 335.7448905683720568, 15.47720386886985366 ) ) ;
#15513 = CARTESIAN_POINT ( 'NONE',  ( -11.93348319268873503, 470.6823905683720568, -3.332260488124732856 ) ) ;
#15514 = LINE ( 'NONE', #15199, #11294 ) ;
#15515 = CARTESIAN_POINT ( 'NONE',  ( -43.68588794268869435, 200.1437886375728965, 2.403080215999224424E-15 ) ) ;
#15516 = CARTESIAN_POINT ( 'NONE',  ( -32.66413529028186247, 305.0573905601784190, -19.99999999999999289 ) ) ;
#15517 = CARTESIAN_POINT ( 'NONE',  ( -40.53162694259544452, 394.1198905683720000, -11.84573899990672707 ) ) ;
#15518 = DIRECTION ( 'NONE',  ( 0.000000000000000000, 1.224646799147353207E-16, 1.000000000000000000 ) ) ;
#15519 = CARTESIAN_POINT ( 'NONE',  ( -8.685887942688742314, 521.9323905601785327, 3.978247347593161010 ) ) ;
#15520 = CARTESIAN_POINT ( 'NONE',  ( -16.84014894278198682, 340.1198905683720568, -11.84573899990672707 ) ) ;
#15521 = AXIS2_PLACEMENT_3D ( 'NONE', #7694, #17547, #4456 ) ;
#15522 = EDGE_CURVE ( 'NONE', #18782, #10285, #19776, .T. ) ;
#15523 = ORIENTED_EDGE ( 'NONE', *, *, #19803, .F. ) ;
#15524 = CARTESIAN_POINT ( 'NONE',  ( -19.19641293061500065, 510.4323905683720000, -14.20200298773971603 ) ) ;
#15525 = ORIENTED_EDGE ( 'NONE', *, *, #10344, .T. ) ;
#15526 = CARTESIAN_POINT ( 'NONE',  ( -8.685887942688719221, 352.5573905601784759, -3.978247347593165895 ) ) ;
#15527 =( BOUNDED_CURVE ( )  B_SPLINE_CURVE ( 2, ( #3425, #12949, #19538, #11313, #19861, #10005, #17907, #1818, #18018, #3212, #9790, #1591, #8162, #720, #10320, #6975, #12060 ),
 .UNSPECIFIED., .F., .T. ) 
 B_SPLINE_CURVE_WITH_KNOTS ( ( 3, 2, 2, 2, 2, 2, 2, 2, 3 ),
 ( 0.7187500000000002220, 0.7207031250000002220, 0.7226562500000002220, 0.7246093750000002220, 0.7265625000000002220, 0.7285156250000003331, 0.7304687500000003331, 0.7324218750000003331, 0.7343750000000003331 ),
 .UNSPECIFIED. ) 
 CURVE ( )  GEOMETRIC_REPRESENTATION_ITEM ( )  RATIONAL_B_SPLINE_CURVE ( ( 0.9999999999999977796, 0.9807852804032326510, 1.000000000000000000, 0.9807852804032304306, 1.000000000000000000, 0.9807852804032304306, 1.000000000000000000, 0.9807852804032304306, 1.000000000000000000, 0.9807852804032304306, 1.000000000000000000, 0.9807852804032304306, 1.000000000000000000, 0.9807852804032304306, 1.000000000000000000, 0.9807852804032270999, 1.000000000000003331 ) ) 
 REPRESENTATION_ITEM ( '' )  );
#15528 = CARTESIAN_POINT ( 'NONE',  ( -21.03221929538692692, 378.8698905765656377, -18.47759065022572855 ) ) ;
#15529 = CARTESIAN_POINT ( 'NONE',  ( -17.35679799567828496, 315.4323905765656946, 16.95518130045146421 ) ) ;
#15530 = FACE_OUTER_BOUND ( 'NONE', #14393, .T. ) ;
#15531 = CARTESIAN_POINT ( 'NONE',  ( -8.685887942688736985, 492.2448905601785327, -2.449293598294705724E-15 ) ) ;
#15532 = CARTESIAN_POINT ( 'NONE',  ( -14.48388495494900852, 467.9323905683721136, 9.489475012073732785 ) ) ;
#15533 = ORIENTED_EDGE ( 'NONE', *, *, #17728, .F. ) ;
#15534 = CARTESIAN_POINT ( 'NONE',  ( -11.93348319268873503, 479.1823905683720568, -3.332260488124732856 ) ) ;
#15535 = CARTESIAN_POINT ( 'NONE',  ( -14.54375231895775222, 250.9948905601784759, 14.14213562373094568 ) ) ;
#15536 = CARTESIAN_POINT ( 'NONE',  ( -8.685887942688726326, 406.9948905765656377, -2.449293598294705724E-15 ) ) ;
#15537 = DIRECTION ( 'NONE',  ( 0.000000000000000000, -1.000000000000000000, 0.000000000000000000 ) ) ;
#15538 = DIRECTION ( 'NONE',  ( 0.000000000000000000, 0.000000000000000000, 1.000000000000000000 ) ) ;
#15539 = CARTESIAN_POINT ( 'NONE',  ( -32.66413529028188378, 485.0573905601785327, -19.99999999999999289 ) ) ;
#15540 =( REPRESENTATION_RELATIONSHIP ('NONE','NONE', #1888, #4076 ) REPRESENTATION_RELATIONSHIP_WITH_TRANSFORMATION ( #4022 )SHAPE_REPRESENTATION_RELATIONSHIP( ) );
#15541 = FACE_OUTER_BOUND ( 'NONE', #1032, .T. ) ;
#15542 = VECTOR ( 'NONE', #10270, 1000.000000000000000 ) ;
#15543 = EDGE_CURVE ( 'NONE', #10281, #13852, #4962, .T. ) ;
#15544 = CARTESIAN_POINT ( 'NONE',  ( 20.42502041961813930, 230.5765313837437418, -40.00000000000000000 ) ) ;
#15545 = CYLINDRICAL_SURFACE ( 'NONE', #11123, 175.0000000000000284 ) ;
#15546 = DIRECTION ( 'NONE',  ( -1.000000000000000000, 0.000000000000000000, 0.000000000000000000 ) ) ;
#15547 = CARTESIAN_POINT ( 'NONE',  ( -40.53162694259543031, 286.6198905683720000, 11.84573899990672885 ) ) ;
#15548 = CARTESIAN_POINT ( 'NONE',  ( -45.64106924314017277, 256.3073905601784759, -11.32908994701042715 ) ) ;
#15549 = CARTESIAN_POINT ( 'NONE',  ( -8.685887942688859553, 406.6823905765655809, 3.978247347593479866 ) ) ;
#15550 = CARTESIAN_POINT ( 'NONE',  ( -25.35362745456399125, 448.1823905683719431, 16.75240474999998952 ) ) ;
#15551 = CARTESIAN_POINT ( 'NONE',  ( -32.66413529028186957, 329.8073905765655809, -19.99999999999999289 ) ) ;
#15552 = CARTESIAN_POINT ( 'NONE',  ( -16.84014894278197971, 261.6198905683720568, -11.84573899990672707 ) ) ;
#15553 = EDGE_CURVE ( 'NONE', #9225, #20381, #20303, .T. ) ;
#15554 = ORIENTED_EDGE ( 'NONE', *, *, #16571, .F. ) ;
#15555 = CARTESIAN_POINT ( 'NONE',  ( -24.70764059509557242, 479.1823905765656377, -19.99999999999999289 ) ) ;
#15556 = ORIENTED_EDGE ( 'NONE', *, *, #8233, .T. ) ;
#15557 = CARTESIAN_POINT ( 'NONE',  ( -22.27502019258949062, 488.4948905683720568, 15.47720386886985189 ) ) ;
#15558 = ORIENTED_EDGE ( 'NONE', *, *, #15142, .F. ) ;
#15559 = LINE ( 'NONE', #12405, #14900 ) ;
#15560 = CARTESIAN_POINT ( 'NONE',  ( -13.20868407381884779, 249.4948905683720284, -6.410867750099233042 ) ) ;
#15561 = VERTEX_POINT ( 'NONE', #6150 ) ;
#15562 = DIRECTION ( 'NONE',  ( 1.000000000000000000, 0.000000000000000000, 0.000000000000000000 ) ) ;
#15563 = CARTESIAN_POINT ( 'NONE',  ( -21.03221929538692336, 465.1198905765655809, 18.47759065022572500 ) ) ;
#15564 = LINE ( 'NONE', #3969, #9269 ) ;
#15565 = CARTESIAN_POINT ( 'NONE',  ( 75.04415151326509203, 162.3117964647028373, 60.96179693900064933 ) ) ;
#15566 = DIRECTION ( 'NONE',  ( -1.250996701150283068E-16, 1.000000000000000000, 0.000000000000000000 ) ) ;
#15567 = CARTESIAN_POINT ( 'NONE',  ( -14.48388495494901740, 521.3073905683720568, -9.489475012073736337 ) ) ;
#15568 = DIRECTION ( 'NONE',  ( -0.000000000000000000, 1.000000000000000000, -0.000000000000000000 ) ) ;
#15569 = CARTESIAN_POINT ( 'NONE',  ( -38.17536295476244135, 242.3073905683720284, -14.20200298773971426 ) ) ;
#15570 = CARTESIAN_POINT ( 'NONE',  ( -13.20868407381885667, 339.7448905683720568, 6.410867750099229490 ) ) ;
#15571 = CARTESIAN_POINT ( 'NONE',  ( -32.66413529028186247, 319.4323905601785327, 19.99999999999999289 ) ) ;
#15572 = VECTOR ( 'NONE', #13461, 1000.000000000000000 ) ;
#15573 = CARTESIAN_POINT ( 'NONE',  ( -45.64106924314017277, 272.9323905765655809, 11.32908994701042538 ) ) ;
#15574 = CARTESIAN_POINT ( 'NONE',  ( -16.84014894278199748, 410.1198905683720000, -11.84573899990672707 ) ) ;
#15575 = CARTESIAN_POINT ( 'NONE',  ( -32.66413529028186247, 324.1823905765655809, 19.99999999999999289 ) ) ;
#15576 = EDGE_CURVE ( 'NONE', #11573, #6728, #16120, .T. ) ;
#15577 = CARTESIAN_POINT ( 'NONE',  ( -42.82802356641966668, 395.9948905601784759, -14.14213562373094746 ) ) ;
#15578 = EDGE_CURVE ( 'NONE', #6060, #19853, #14783, .T. ) ;
#15579 = ORIENTED_EDGE ( 'NONE', *, *, #4761, .F. ) ;
#15580 = DIRECTION ( 'NONE',  ( -0.000000000000000000, -0.000000000000000000, 1.000000000000000000 ) ) ;
#15581 = ORIENTED_EDGE ( 'NONE', *, *, #19135, .T. ) ;
#15582 = VERTEX_POINT ( 'NONE', #8414 ) ;
#15583 = CARTESIAN_POINT ( 'NONE',  ( -38.17536295476246977, 503.8073905683721136, -14.20200298773971426 ) ) ;
#15584 = DIRECTION ( 'NONE',  ( 1.000000000000000000, 0.000000000000000000, 0.000000000000000000 ) ) ;
#15585 = VECTOR ( 'NONE', #854, 1000.000000000000000 ) ;
#15586 = ORIENTED_EDGE ( 'NONE', *, *, #5509, .T. ) ;
#15587 = CARTESIAN_POINT ( 'NONE',  ( -45.43829269268870519, 305.0573905683720000, -3.332260488124726638 ) ) ;
#15588 = PRODUCT_DEFINITION_FORMATION_WITH_SPECIFIED_SOURCE ( 'ANY', '', #4407, .NOT_KNOWN. ) ;
#15589 = ORIENTED_EDGE ( 'NONE', *, *, #4453, .F. ) ;
#15590 = CARTESIAN_POINT ( 'NONE',  ( -22.27502019258947641, 346.9948905683720000, 15.47720386886985189 ) ) ;
#15591 = CARTESIAN_POINT ( 'NONE',  ( -35.09675569278795138, 345.7448905683720568, 15.47720386886985366 ) ) ;
#15592 = AXIS2_PLACEMENT_3D ( 'NONE', #13922, #20510, #7186 ) ;
#15593 = CARTESIAN_POINT ( 'NONE',  ( -40.01497788969913216, 280.4323905765655809, -16.95518130045146421 ) ) ;
#15594 = AXIS2_PLACEMENT_3D ( 'NONE', #4462, #17551, #12902 ) ;
#15595 = CARTESIAN_POINT ( 'NONE',  ( -40.53162694259542320, 255.1198905683720284, 11.84573899990672885 ) ) ;
#15596 = CARTESIAN_POINT ( 'NONE',  ( -43.59942232657301986, 200.4092789822994405, 1.616039188923344083 ) ) ;
#15597 = CARTESIAN_POINT ( 'NONE',  ( -35.09675569278795138, 393.4948905683720000, -15.47720386886985544 ) ) ;
#15598 = LINE ( 'NONE', #4435, #10608 ) ;
#15599 = CARTESIAN_POINT ( 'NONE',  ( 52.60622592008805043, 30.52886280891152282, -151.0302712373927250 ) ) ;
#15600 = DIRECTION ( 'NONE',  ( 1.000000000000000000, 0.000000000000000000, 0.000000000000000000 ) ) ;
#15601 = CARTESIAN_POINT ( 'NONE',  ( -28.68588794268870856, 312.8698905683720000, -16.75240474999999307 ) ) ;
#15602 = CARTESIAN_POINT ( 'NONE',  ( -44.16309181155858710, 463.2448905683720568, -6.410867750099231266 ) ) ;
#15603 = VERTEX_POINT ( 'NONE', #15544 ) ;
#15604 = CARTESIAN_POINT ( 'NONE',  ( -48.68588794268871567, 447.5573905601784759, 3.978247347593168115 ) ) ;
#15605 = CARTESIAN_POINT ( 'NONE',  ( -25.35362745456398059, 281.0573905683720568, -16.75240474999999307 ) ) ;
#15606 = ORIENTED_EDGE ( 'NONE', *, *, #1234, .F. ) ;
#15607 = VERTEX_POINT ( 'NONE', #13919 ) ;
#15608 = VERTEX_POINT ( 'NONE', #223 ) ;
#15609 = CARTESIAN_POINT ( 'NONE',  ( -3.697298814765020980E-16, -0.6346842323187746882, -6.500000000000000000 ) ) ;
#15610 = CARTESIAN_POINT ( 'NONE',  ( -22.27502019258947996, 300.7448905683720568, -15.47720386886985544 ) ) ;
#15611 = CARTESIAN_POINT ( 'NONE',  ( -42.88789093042843348, 366.3073905683720000, 9.489475012073734561 ) ) ;
#15612 = CARTESIAN_POINT ( 'NONE',  ( -47.16347859291443712, 296.6198905601784759, -7.653668647301793193 ) ) ;
#15613 = CARTESIAN_POINT ( 'NONE',  ( -11.73070664223726567, 516.0573905765655809, 11.32908994701042005 ) ) ;
#15614 = CARTESIAN_POINT ( 'NONE',  ( -44.16309181155857289, 394.4948905683720000, 6.410867750099241924 ) ) ;
#15615 = CARTESIAN_POINT ( 'NONE',  ( -35.09675569278793716, 237.2448905683720000, 15.47720386886985366 ) ) ;
#15616 = CARTESIAN_POINT ( 'NONE',  ( -45.43829269268871940, 413.5573905683720000, -3.332260488124726638 ) ) ;
#15617 = CARTESIAN_POINT ( 'NONE',  ( -14.54375231895776821, 348.2448905765656377, -14.14213562373094746 ) ) ;
#15618 = DIRECTION ( 'NONE',  ( -1.000000000000000000, -0.000000000000000000, -0.000000000000000000 ) ) ;
#15619 = CARTESIAN_POINT ( 'NONE',  ( -40.53162694259543031, 315.1198905683720568, 11.84573899990672885 ) ) ;
#15620 =( NAMED_UNIT ( * ) SI_UNIT ( $, .STERADIAN. ) SOLID_ANGLE_UNIT ( ) );
#15621 = CARTESIAN_POINT ( 'NONE',  ( -42.88789093042844769, 466.3073905683720568, 9.489475012073736337 ) ) ;
#15622 = DIRECTION ( 'NONE',  ( -0.000000000000000000, -0.000000000000000000, -1.000000000000000000 ) ) ;
#15623 = CARTESIAN_POINT ( 'NONE',  ( 4.700000000000000178, 0.000000000000000000, 0.000000000000000000 ) ) ;
#15624 = VECTOR ( 'NONE', #8183, 1000.000000000000000 ) ;
#15625 = CARTESIAN_POINT ( 'NONE',  ( -10.20829729246297113, 226.3698905765656377, 7.653668647301790529 ) ) ;
#15626 = CIRCLE ( 'NONE', #1461, 15.00000000000000355 ) ;
#15627 = CARTESIAN_POINT ( 'NONE',  ( -44.16309181155857289, 374.7448905683720568, -6.410867750099231266 ) ) ;
#15628 = FACE_OUTER_BOUND ( 'NONE', #2562, .T. ) ;
#15629 = B_SPLINE_CURVE_WITH_KNOTS ( 'NONE', 3,
 ( #1457, #16282, #12922, #3399, #19511, #1564, #11502, #2976, #8246, #19723, #14765, #21138, #4690, #11612, #11182, #9764, #11284, #21244, #5012, #8134, #16493, #14552, #6738, #6409, #13023, #9980, #19615, #21351, #1675, #9554, #14875, #19836, #18203, #4792 ),
 .UNSPECIFIED., .F., .F.,
 ( 4, 2, 2, 2, 2, 2, 2, 2, 2, 2, 2, 2, 2, 2, 2, 2, 4 ),
 ( 0.01132186211905188838, 0.01210437382053968641, 0.01288688552202748618, 0.01445190892500309264, 0.01523442062649089240, 0.01601693232797869390, 0.01758195573095429343, 0.01914697913392988948, 0.02071200253690548554, 0.02227702593988108160, 0.02384204934285668112, 0.02697209614880787670, 0.03010214295475907922, 0.03166716635773467875, 0.03323218976071028175, 0.03479721316368587780, 0.03636223656666148080 ),
 .UNSPECIFIED. ) ;
#15630 = EDGE_CURVE ( 'NONE', #9671, #4636, #18722, .T. ) ;
#15631 = CARTESIAN_POINT ( 'NONE',  ( -48.68588794268872988, 516.9323905601784190, -3.978247347593158345 ) ) ;
#15632 = CARTESIAN_POINT ( 'NONE',  ( -45.43829269268870519, 334.1823905683720000, 3.332260488124734632 ) ) ;
#15633 = ORIENTED_EDGE ( 'NONE', *, *, #923, .T. ) ;
#15634 = CARTESIAN_POINT ( 'NONE',  ( -16.84014894278200813, 500.1198905683720000, -11.84573899990672707 ) ) ;
#15635 = VERTEX_POINT ( 'NONE', #2239 ) ;
#15636 = CARTESIAN_POINT ( 'NONE',  ( -48.68588794268854514, 381.6823905765656377, -3.978247347593583783 ) ) ;
#15637 = FACE_OUTER_BOUND ( 'NONE', #5718, .T. ) ;
#15638 = DIRECTION ( 'NONE',  ( 0.000000000000000000, 0.000000000000000000, 1.000000000000000000 ) ) ;
#15639 = CARTESIAN_POINT ( 'NONE',  ( -48.68588794268869435, 231.9948905765656377, 0.000000000000000000 ) ) ;
#15640 = CARTESIAN_POINT ( 'NONE',  ( -38.17536295476246266, 465.4323905683720000, 14.20200298773971781 ) ) ;
#15641 = AXIS2_PLACEMENT_3D ( 'NONE', #15248, #434, #7001 ) ;
#15642 = VERTEX_POINT ( 'NONE', #12064 ) ;
#15643 = CARTESIAN_POINT ( 'NONE',  ( -40.53162694259545162, 492.6198905683720000, -11.84573899990672707 ) ) ;
#15644 = CARTESIAN_POINT ( 'NONE',  ( -14.54375231895775222, 245.7448905765656093, 14.14213562373094568 ) ) ;
#15645 = CARTESIAN_POINT ( 'NONE',  ( -47.16347859291445133, 412.6198905765656377, 7.653668647301805628 ) ) ;
#15646 = CARTESIAN_POINT ( 'NONE',  ( -11.73070664223724080, 277.9323905765655809, -11.32908994701042538 ) ) ;
#15647 = DIRECTION ( 'NONE',  ( -1.191790137725560488E-16, 1.000000000000000000, -0.000000000000000000 ) ) ;
#15648 = CARTESIAN_POINT ( 'NONE',  ( 20.42502041961813930, 230.5765313837437418, 60.00000000000000000 ) ) ;
#15649 = LINE ( 'NONE', #14130, #6638 ) ;
#15650 = EDGE_CURVE ( 'NONE', #15664, #16862, #5436, .T. ) ;
#15651 = CARTESIAN_POINT ( 'NONE',  ( -14.54375231895775755, 258.2448905765656377, -14.14213562373094746 ) ) ;
#15652 = CARTESIAN_POINT ( 'NONE',  ( 158.8141120573112630, 620.7448905601785327, 0.000000000000000000 ) ) ;
#15653 = CARTESIAN_POINT ( 'NONE',  ( 43.53705524234220547, 56.85652257517428865, -96.62835994548002816 ) ) ;
#15654 = AXIS2_PLACEMENT_3D ( 'NONE', #21167, #4823, #11213 ) ;
#15655 = CARTESIAN_POINT ( 'NONE',  ( -44.16309181155856578, 284.7448905683720568, -6.410867750099231266 ) ) ;
#15656 = CARTESIAN_POINT ( 'NONE',  ( -28.68588794268872633, 378.8848358243226357, 0.000000000000000000 ) ) ;
#15657 = CARTESIAN_POINT ( 'NONE',  ( -32.01814843081345430, 437.5573905683720000, 16.75240474999999307 ) ) ;
#15658 = CARTESIAN_POINT ( 'NONE',  ( -45.43829269268869808, 265.3698905683720000, 0.000000000000000000 ) ) ;
#15659 = ORIENTED_EDGE ( 'NONE', *, *, #1809, .F. ) ;
#15660 = LINE ( 'NONE', #5583, #19818 ) ;
#15661 = ORIENTED_EDGE ( 'NONE', *, *, #15458, .F. ) ;
#15662 = CARTESIAN_POINT ( 'NONE',  ( -14.48388495494901029, 479.4323905683720568, 9.489475012073731008 ) ) ;
#15663 = EDGE_CURVE ( 'NONE', #10452, #6038, #7080, .T. ) ;
#15664 = VERTEX_POINT ( 'NONE', #13701 ) ;
#15665 = DIRECTION ( 'NONE',  ( -1.000000000000000000, 0.000000000000000000, 0.000000000000000000 ) ) ;
#15666 = CARTESIAN_POINT ( 'NONE',  ( -16.84014894278197261, 247.6198905683720284, 11.84573899990672530 ) ) ;
#15667 = CIRCLE ( 'NONE', #3895, 21.20245194746113526 ) ;
#15668 = ORIENTED_EDGE ( 'NONE', *, *, #3720, .T. ) ;
#15669 = LINE ( 'NONE', #10986, #16276 ) ;
#15670 = CARTESIAN_POINT ( 'NONE',  ( -24.70764059509557597, 469.1823905765656377, -19.99999999999999289 ) ) ;
#15671 = CARTESIAN_POINT ( 'NONE',  ( 158.8141120573112630, 10.52886280891152104, 10.00000000000000888 ) ) ;
#15672 = CARTESIAN_POINT ( 'NONE',  ( 158.8141120573112630, 400.5398297725602674, -9.999999999999994671 ) ) ;
#15673 = CARTESIAN_POINT ( 'NONE',  ( -25.35362745456396283, 228.1823905683720284, 16.75240474999998952 ) ) ;
#15674 = EDGE_CURVE ( 'NONE', #12962, #5244, #11669, .T. ) ;
#15675 = CARTESIAN_POINT ( 'NONE',  ( -19.19641293061500065, 511.9323905683721136, -14.20200298773971603 ) ) ;
#15676 = DIRECTION ( 'NONE',  ( -1.191790137725560488E-16, 1.000000000000000000, -0.000000000000000000 ) ) ;
#15677 = CARTESIAN_POINT ( 'NONE',  ( -14.48388495494898542, 239.8073905683720284, -9.489475012073736337 ) ) ;
#15678 = CARTESIAN_POINT ( 'NONE',  ( -44.16309181155857289, 334.7448905683720568, -6.410867750099231266 ) ) ;
#15679 = DIRECTION ( 'NONE',  ( 0.000000000000000000, 0.000000000000000000, 1.000000000000000000 ) ) ;
#15680 = CARTESIAN_POINT ( 'NONE',  ( -36.33955658999050797, 303.8698905765656377, 18.47759065022572500 ) ) ;
#15681 = CIRCLE ( 'NONE', #2550, 220.7252770684331438 ) ;
#15682 = CARTESIAN_POINT ( 'NONE',  ( -45.43829269268871229, 393.5573905683720568, -3.332260488124726194 ) ) ;
#15683 = CARTESIAN_POINT ( 'NONE',  ( -45.43829269268873361, 535.3698905683720568, 0.000000000000000000 ) ) ;
#15684 = CARTESIAN_POINT ( 'NONE',  ( -47.16347859291444422, 386.6198905601784759, -7.653668647301793193 ) ) ;
#15685 = VERTEX_POINT ( 'NONE', #19889 ) ;
#15686 = PLANE ( 'NONE',  #12206 ) ;
#15687 = VERTEX_POINT ( 'NONE', #111 ) ;
#15688 = ORIENTED_EDGE ( 'NONE', *, *, #21318, .F. ) ;
#15689 = CARTESIAN_POINT ( 'NONE',  ( -11.93348319268873858, 510.6823905683720000, -3.332260488124732856 ) ) ;
#15690 = CARTESIAN_POINT ( 'NONE',  ( -48.68588794268870146, 291.9948905765656377, 0.000000000000000000 ) ) ;
#15691 = ORIENTED_EDGE ( 'NONE', *, *, #14401, .F. ) ;
#15692 = CARTESIAN_POINT ( 'NONE',  ( -22.27502019258946930, 298.4948905683720568, 15.47720386886985189 ) ) ;
#15693 = ORIENTED_EDGE ( 'NONE', *, *, #12732, .F. ) ;
#15694 = CARTESIAN_POINT ( 'NONE',  ( -28.68588794268870856, 336.3698905683720000, 16.75240474999999307 ) ) ;
#15695 = CARTESIAN_POINT ( 'NONE',  ( -38.17536295476245556, 342.3073905683721136, -14.20200298773971426 ) ) ;
#15696 = AXIS2_PLACEMENT_3D ( 'NONE', #2931, #7778, #3248 ) ;
#15697 = CARTESIAN_POINT ( 'NONE',  ( -32.66413529028186957, 279.8073905765655809, -19.99999999999999289 ) ) ;
#15698 = DIRECTION ( 'NONE',  ( 1.000000000000000000, 0.000000000000000000, 0.000000000000000000 ) ) ;
#15699 = CARTESIAN_POINT ( 'NONE',  ( -11.93348319268870661, 239.1823905683720284, -3.332260488124732856 ) ) ;
#15700 = CARTESIAN_POINT ( 'NONE',  ( -42.93765923600279422, 203.3731313234726201, 4.678819197459195500 ) ) ;
#15701 = CARTESIAN_POINT ( 'NONE',  ( -44.16309181155857999, 394.7448905683720568, -6.410867750099231266 ) ) ;
#15702 = DIRECTION ( 'NONE',  ( -1.000000000000000000, -0.000000000000000000, -0.000000000000000000 ) ) ;
#15703 = CARTESIAN_POINT ( 'NONE',  ( -36.33955658999052218, 450.1198905765655809, -18.47759065022572855 ) ) ;
#15704 = CARTESIAN_POINT ( 'NONE',  ( -40.01497788969916058, 510.4323905765656377, -16.95518130045146421 ) ) ;
#15705 = CARTESIAN_POINT ( 'NONE',  ( -45.43829269268871229, 433.5573905683719431, -3.332260488124726194 ) ) ;
#15706 = VERTEX_POINT ( 'NONE', #20294 ) ;
#15707 = CARTESIAN_POINT ( 'NONE',  ( -8.685887942688731655, 451.9323905601784759, 3.978247347593161010 ) ) ;
#15708 = EDGE_CURVE ( 'NONE', #1471, #74, #5464, .T. ) ;
#15709 = VERTEX_POINT ( 'NONE', #13304 ) ;
#15710 = CARTESIAN_POINT ( 'NONE',  ( 40.42502041961814996, 170.1716627696692683, -40.00000000000000000 ) ) ;
#15711 = VERTEX_POINT ( 'NONE', #8920 ) ;
#15712 = ORIENTED_EDGE ( 'NONE', *, *, #16152, .F. ) ;
#15713 = CARTESIAN_POINT ( 'NONE',  ( 0.2565376335216141834, -2.516992571280034507, -6.499999999999999112 ) ) ;
#15714 = CARTESIAN_POINT ( 'NONE',  ( -45.64106924314017988, 318.1823905601784759, 11.32908994701042715 ) ) ;
#15715 = ADVANCED_FACE ( 'NONE', ( #11561 ), #3846, .T. ) ;
#15716 = CARTESIAN_POINT ( 'NONE',  ( -38.17536295476244135, 295.4323905683720000, 14.20200298773971781 ) ) ;
#15717 = EDGE_CURVE ( 'NONE', #16350, #12966, #2448, .T. ) ;
#15718 = CARTESIAN_POINT ( 'NONE',  ( -35.09675569278795138, 357.2448905683720000, 15.47720386886985366 ) ) ;
#15719 = DIRECTION ( 'NONE',  ( 0.000000000000000000, 1.000000000000000000, -0.000000000000000000 ) ) ;
#15720 = CARTESIAN_POINT ( 'NONE',  ( -40.01497788969915348, 523.5573905765655809, 16.95518130045146776 ) ) ;
#15721 = CARTESIAN_POINT ( 'NONE',  ( -22.27502019258947996, 396.9948905683720568, 15.47720386886985189 ) ) ;
#15722 = CARTESIAN_POINT ( 'NONE',  ( -38.17536295476244135, 243.8073905683720284, -14.20200298773971426 ) ) ;
#15723 = CARTESIAN_POINT ( 'NONE',  ( -45.43829269268871940, 413.8698905683720568, 0.000000000000000000 ) ) ;
#15724 = CARTESIAN_POINT ( 'NONE',  ( -28.68588794268871567, 349.4948905765656377, -19.99999999999999289 ) ) ;
#15725 = FACE_OUTER_BOUND ( 'NONE', #9569, .T. ) ;
#15726 = CARTESIAN_POINT ( 'NONE',  ( -45.43829269268870519, 304.1823905683720568, 3.332260488124734632 ) ) ;
#15727 = SHAPE_REPRESENTATION_RELATIONSHIP ( 'NONE' , 'NONE' ,  #4206, #11515 ) ;
#15728 = CARTESIAN_POINT ( 'NONE',  ( -42.88789093042844769, 464.4323905683720000, -9.489475012073736337 ) ) ;
#15729 = EDGE_CURVE ( 'NONE', #6455, #7334, #20398, .T. ) ;
#15730 = CARTESIAN_POINT ( 'NONE',  ( -48.68588794268878672, 512.3073905765656946, 3.978247347593061978 ) ) ;
#15731 = LINE ( 'NONE', #4031, #3840 ) ;
#15732 = FACE_OUTER_BOUND ( 'NONE', #18009, .T. ) ;
#15733 = CARTESIAN_POINT ( 'NONE',  ( -28.68588794268871567, 362.8698905683720000, -16.75240474999999307 ) ) ;
#15734 = DIRECTION ( 'NONE',  ( 0.000000000000000000, 1.000000000000000000, -0.000000000000000000 ) ) ;
#15735 = CARTESIAN_POINT ( 'NONE',  ( -45.64106924314020119, 508.1823905601784759, 11.32908994701042715 ) ) ;
#15736 = CARTESIAN_POINT ( 'NONE',  ( -11.93348319268872260, 348.5573905683720000, 3.332260488124728415 ) ) ;
#15737 = VERTEX_POINT ( 'NONE', #12285 ) ;
#15738 = CARTESIAN_POINT ( 'NONE',  ( -38.17536295476246977, 505.4323905683720568, 14.20200298773971781 ) ) ;
#15739 = ORIENTED_EDGE ( 'NONE', *, *, #8289, .T. ) ;
#15740 = CARTESIAN_POINT ( 'NONE',  ( -24.70764059509556176, 354.4323905601784759, -19.99999999999999289 ) ) ;
#15741 = CARTESIAN_POINT ( 'NONE',  ( -10.20829729246298001, 316.3698905765656377, 7.653668647301790529 ) ) ;
#15742 = CARTESIAN_POINT ( 'NONE',  ( -19.19641293061498999, 421.9323905683720000, -14.20200298773971603 ) ) ;
#15743 = CARTESIAN_POINT ( 'NONE',  ( -36.33955658999050087, 290.1198905765656377, -18.47759065022572855 ) ) ;
#15744 = FACE_OUTER_BOUND ( 'NONE', #7553, .T. ) ;
#15745 = CARTESIAN_POINT ( 'NONE',  ( -35.09675569278796559, 465.7448905683720568, 15.47720386886985366 ) ) ;
#15746 = ORIENTED_EDGE ( 'NONE', *, *, #2098, .F. ) ;
#15747 = CARTESIAN_POINT ( 'NONE',  ( -28.68588794268872988, 471.3698905683720568, -16.75240474999999307 ) ) ;
#15748 = CARTESIAN_POINT ( 'NONE',  ( 0.05533025579362052526, 4.993776679985852951, 4.350525068611870161 ) ) ;
#15749 = CARTESIAN_POINT ( 'NONE',  ( -28.68588794268871567, 394.4948905765656377, 19.99999999999999289 ) ) ;
#15750 = LINE ( 'NONE', #5996, #11003 ) ;
#15751 = CARTESIAN_POINT ( 'NONE',  ( -17.35679799567829562, 368.5573905765655809, -16.95518130045146421 ) ) ;
#15752 = CARTESIAN_POINT ( 'NONE',  ( -8.685887942688728103, 416.9948905765656377, -2.449293598294705724E-15 ) ) ;
#15753 = CARTESIAN_POINT ( 'NONE',  ( 158.8141120573112630, 400.5398297725603243, 0.000000000000000000 ) ) ;
#15754 = DIRECTION ( 'NONE',  ( -0.02283316540262222277, 0.9997392892938120612, 0.000000000000000000 ) ) ;
#15755 = LINE ( 'NONE', #4280, #7665 ) ;
#15756 = LINE ( 'NONE', #18556, #20079 ) ;
#15757 = CARTESIAN_POINT ( 'NONE',  ( -13.20868407381885135, 280.9948905683720000, -6.410867750099233042 ) ) ;
#15758 = CARTESIAN_POINT ( 'NONE',  ( -10.20829729246297291, 252.8698905601785043, -7.653668647301794969 ) ) ;
#15759 = DIRECTION ( 'NONE',  ( 0.000000000000000000, 0.000000000000000000, -1.000000000000000000 ) ) ;
#15760 = CARTESIAN_POINT ( 'NONE',  ( -45.43829269268871229, 435.0573905683720568, -3.332260488124726194 ) ) ;
#15761 = CARTESIAN_POINT ( 'NONE',  ( -21.03221929538692692, 398.8698905765656377, -18.47759065022572855 ) ) ;
#15762 = CARTESIAN_POINT ( 'NONE',  ( -11.93348319268871016, 260.0573905683720000, 3.332260488124728415 ) ) ;
#15763 = ORIENTED_EDGE ( 'NONE', *, *, #12390, .F. ) ;
#15764 = CARTESIAN_POINT ( 'NONE',  ( -8.685887942688605534, 477.3073905765656377, -3.978247347592846594 ) ) ;
#15765 = ORIENTED_EDGE ( 'NONE', *, *, #3408, .T. ) ;
#15766 = CARTESIAN_POINT ( 'NONE',  ( -45.43829269268872650, 485.6823905683721136, 3.332260488124734632 ) ) ;
#15767 = ADVANCED_FACE ( 'NONE', ( #18148 ), #6684, .F. ) ;
#15768 = ORIENTED_EDGE ( 'NONE', *, *, #20375, .F. ) ;
#15769 = CARTESIAN_POINT ( 'NONE',  ( -8.685887942688456320, 362.5573905601784190, -3.978247347592526850 ) ) ;
#15770 = CARTESIAN_POINT ( 'NONE',  ( -38.17536295476244135, 232.3073905683720568, -14.20200298773971426 ) ) ;
#15771 = ORIENTED_EDGE ( 'NONE', *, *, #6434, .F. ) ;
#15772 = CARTESIAN_POINT ( 'NONE',  ( -28.68588794268873698, 521.3698905683720568, -16.75240474999999307 ) ) ;
#15773 = DIRECTION ( 'NONE',  ( 1.000000000000000000, 0.000000000000000000, 0.000000000000000000 ) ) ;
#15774 = AXIS2_PLACEMENT_3D ( 'NONE', #7480, #1229, #2742 ) ;
#15775 = CARTESIAN_POINT ( 'NONE',  ( -45.64106924314020119, 471.0573905765656377, -11.32908994701042715 ) ) ;
#15776 = CARTESIAN_POINT ( 'NONE',  ( -8.685887942688809815, 351.9323905601785327, 3.978247347593374172 ) ) ;
#15777 = ADVANCED_FACE ( 'NONE', ( #17467, #4594 ), #19305, .T. ) ;
#15778 = DIRECTION ( 'NONE',  ( 0.000000000000000000, 0.000000000000000000, 1.000000000000000000 ) ) ;
#15779 = CARTESIAN_POINT ( 'NONE',  ( -10.20829729246299600, 452.8698905601785327, -7.653668647301794969 ) ) ;
#15780 = CARTESIAN_POINT ( 'NONE',  ( -40.53162694259542320, 226.6198905683720000, 11.84573899990672885 ) ) ;
#15781 = VECTOR ( 'NONE', #11592, 1000.000000000000000 ) ;
#15782 = CARTESIAN_POINT ( 'NONE',  ( -19.19641293061499709, 508.8073905683720000, 14.20200298773971426 ) ) ;
#15783 = DIRECTION ( 'NONE',  ( 0.9997392892938121722, 0.02283316540262222971, -0.000000000000000000 ) ) ;
#15784 = CARTESIAN_POINT ( 'NONE',  ( -45.43829269268869098, 244.1823905683720568, 3.332260488124734632 ) ) ;
#15785 = CARTESIAN_POINT ( 'NONE',  ( -32.01814843081344719, 337.5573905683720000, 16.75240474999999307 ) ) ;
#15786 = CARTESIAN_POINT ( 'NONE',  ( 29.72350413846044859, 280.4463447002762564, 40.00000000000000000 ) ) ;
#15787 = CARTESIAN_POINT ( 'NONE',  ( -48.68588794268880093, 357.5573905601784190, 3.978247347592954952 ) ) ;
#15788 = VECTOR ( 'NONE', #14775, 1000.000000000000114 ) ;
#15789 = CARTESIAN_POINT ( 'NONE',  ( -25.35362745456398414, 386.6823905683720568, 16.75240474999998952 ) ) ;
#15790 = CARTESIAN_POINT ( 'NONE',  ( -8.685887942688713892, 223.9102039777116886, 2.449293598294704541E-15 ) ) ;
#15791 = CARTESIAN_POINT ( 'NONE',  ( -14.54375231895777176, 383.4948905601784759, -14.14213562373094746 ) ) ;
#15792 = ADVANCED_FACE ( 'NONE', ( #14558 ), #12713, .T. ) ;
#15793 = VECTOR ( 'NONE', #2657, 1000.000000000000000 ) ;
#15794 = ORIENTED_EDGE ( 'NONE', *, *, #7094, .T. ) ;
#15795 = CARTESIAN_POINT ( 'NONE',  ( -40.01497788969914637, 405.6823905601785327, -16.95518130045146421 ) ) ;
#15796 = EDGE_LOOP ( 'NONE', ( #12517, #21150, #9234, #21044, #2748, #14227 ) ) ;
#15797 = ORIENTED_EDGE ( 'NONE', *, *, #4148, .T. ) ;
#15798 = CARTESIAN_POINT ( 'NONE',  ( -16.84014894278200458, 499.1198905683720000, 11.84573899990672530 ) ) ;
#15799 = DIRECTION ( 'NONE',  ( -0.4627175328665442677, 0.000000000000000000, -0.8865057725575725689 ) ) ;
#15800 = VERTEX_POINT ( 'NONE', #12503 ) ;
#15801 = CARTESIAN_POINT ( 'NONE',  ( -44.16309181155856578, 304.7448905683720568, -6.410867750099231266 ) ) ;
#15802 = ORIENTED_EDGE ( 'NONE', *, *, #10096, .F. ) ;
#15803 = CARTESIAN_POINT ( 'NONE',  ( -40.53162694259543741, 332.6198905683720000, -11.84573899990672707 ) ) ;
#15804 = CARTESIAN_POINT ( 'NONE',  ( -42.88789093042843348, 352.9323905683721136, -9.489475012073734561 ) ) ;
#15805 = AXIS2_PLACEMENT_3D ( 'NONE', #5039, #14691, #13383 ) ;
#15806 = CARTESIAN_POINT ( 'NONE',  ( -36.33955658999050797, 283.8698905765656377, 18.47759065022572500 ) ) ;
#15807 = DIRECTION ( 'NONE',  ( 1.000000000000000000, 0.000000000000000000, -0.000000000000000000 ) ) ;
#15808 = CARTESIAN_POINT ( 'NONE',  ( -13.20868407381884602, 238.2448905683720000, 6.410867750099229490 ) ) ;
#15809 = DIRECTION ( 'NONE',  ( 0.000000000000000000, 0.5000000000000004441, -0.8660254037844383745 ) ) ;
#15810 = CARTESIAN_POINT ( 'NONE',  ( -13.20868407381886200, 389.7448905683720000, 6.410867750099229490 ) ) ;
#15811 = EDGE_CURVE ( 'NONE', #17379, #1316, #17369, .T. ) ;
#15812 = AXIS2_PLACEMENT_3D ( 'NONE', #810, #7378, #12364 ) ;
#15813 = DIRECTION ( 'NONE',  ( 0.000000000000000000, 0.000000000000000000, -1.000000000000000000 ) ) ;
#15814 = FACE_OUTER_BOUND ( 'NONE', #11350, .T. ) ;
#15815 = CARTESIAN_POINT ( 'NONE',  ( -21.03221929538690915, 244.1198905601784759, -18.47759065022572855 ) ) ;
#15816 = CARTESIAN_POINT ( 'NONE',  ( -32.01814843081345430, 446.0573905683720568, 16.75240474999999307 ) ) ;
#15817 = VERTEX_POINT ( 'NONE', #15966 ) ;
#15818 = CARTESIAN_POINT ( 'NONE',  ( -48.68588794268871567, 437.5573905601785327, 3.978247347593168115 ) ) ;
#15819 = AXIS2_PLACEMENT_3D ( 'NONE', #3296, #14982, #16283 ) ;
#15820 = DIRECTION ( 'NONE',  ( -1.000000000000000000, -0.000000000000000000, -0.000000000000000000 ) ) ;
#15821 = VERTEX_POINT ( 'NONE', #17576 ) ;
#15822 = VERTEX_POINT ( 'NONE', #12821 ) ;
#15823 = DIRECTION ( 'NONE',  ( 0.000000000000000000, 1.000000000000000000, -0.000000000000000000 ) ) ;
#15824 = CARTESIAN_POINT ( 'NONE',  ( -14.54375231895776466, 323.4948905601784759, -14.14213562373094746 ) ) ;
#15825 = AXIS2_PLACEMENT_3D ( 'NONE', #16977, #18263, #7110 ) ;
#15826 = CARTESIAN_POINT ( 'NONE',  ( -44.16309181155856578, 365.9948905683720568, 6.410867750099241924 ) ) ;
#15827 = CARTESIAN_POINT ( 'NONE',  ( -28.68588794268875120, 585.7448905601785327, 0.000000000000000000 ) ) ;
#15828 = CARTESIAN_POINT ( 'NONE',  ( -42.82802356641968089, 523.2448905765656946, 14.14213562373094923 ) ) ;
#15829 = CARTESIAN_POINT ( 'NONE',  ( -28.68588794268871922, 401.3698905683720000, -16.75240474999999307 ) ) ;
#15830 = CARTESIAN_POINT ( 'NONE',  ( -14.48388495494898365, 239.4323905683720000, 9.489475012073732785 ) ) ;
#15831 = CARTESIAN_POINT ( 'NONE',  ( -40.53162694259544452, 405.1198905683720000, 11.84573899990672885 ) ) ;
#15832 = CARTESIAN_POINT ( 'NONE',  ( -8.685887942688719221, 347.3073905765656377, -3.978247347593165895 ) ) ;
#15833 = CARTESIAN_POINT ( 'NONE',  ( -19.19641293061497578, 310.4323905683720568, -14.20200298773971603 ) ) ;
#15834 = CARTESIAN_POINT ( 'NONE',  ( -28.68588794268872633, 452.8698905683720000, -16.75240474999999307 ) ) ;
#15835 = DIRECTION ( 'NONE',  ( -0.000000000000000000, 1.000000000000000000, -0.000000000000000000 ) ) ;
#15836 = CARTESIAN_POINT ( 'NONE',  ( 0.5805565836007647862, 7.505553499465139389, 2.227827669841787811E-16 ) ) ;
#15837 = CARTESIAN_POINT ( 'NONE',  ( 65.85920792673738333, 170.1716627696692683, -40.00000000000000000 ) ) ;
#15838 = CARTESIAN_POINT ( 'NONE',  ( -35.09675569278794427, 373.4948905683720568, -15.47720386886985544 ) ) ;
#15839 = CARTESIAN_POINT ( 'NONE',  ( -42.88789093042844769, 494.8073905683720000, 9.489475012073736337 ) ) ;
#15840 = SHAPE_REPRESENTATION ( 'Ram Linear Way Guides', ( #12794 ), #718 ) ;
#15841 = CARTESIAN_POINT ( 'NONE',  ( -32.66413529028189089, 499.4323905601784759, 19.99999999999999289 ) ) ;
#15842 = CARTESIAN_POINT ( 'NONE',  ( -44.16309181155856578, 323.2448905683720000, -6.410867750099231266 ) ) ;
#15843 = VERTEX_POINT ( 'NONE', #4279 ) ;
#15844 = CARTESIAN_POINT ( 'NONE',  ( -11.93348319268873858, 508.8698905683719431, -2.051577885510841163E-15 ) ) ;
#15845 = VERTEX_POINT ( 'NONE', #12610 ) ;
#15846 = EDGE_CURVE ( 'NONE', #11996, #15687, #21036, .T. ) ;
#15847 = CARTESIAN_POINT ( 'NONE',  ( -42.82802356641965247, 313.2448905765656377, 14.14213562373094923 ) ) ;
#15848 = VECTOR ( 'NONE', #14567, 1000.000000000000114 ) ;
#15849 = EDGE_CURVE ( 'NONE', #17635, #8154, #19412, .T. ) ;
#15850 = CARTESIAN_POINT ( 'NONE',  ( -45.43829269268871940, 425.3698905683720568, 0.000000000000000000 ) ) ;
#15851 = CARTESIAN_POINT ( 'NONE',  ( -24.70764059509555111, 289.1823905765656377, -19.99999999999999289 ) ) ;
#15852 = CARTESIAN_POINT ( 'NONE',  ( -42.82802356641968089, 520.7448905765656946, -14.14213562373094746 ) ) ;
#15853 = CARTESIAN_POINT ( 'NONE',  ( -44.16309181155857999, 464.4948905683720000, 6.410867750099241924 ) ) ;
#15854 = EDGE_LOOP ( 'NONE', ( #1095, #10682 ) ) ;
#15855 = CARTESIAN_POINT ( 'NONE',  ( -28.68588794268872633, 466.3698905683720000, 16.75240474999999307 ) ) ;
#15856 = CARTESIAN_POINT ( 'NONE',  ( -48.68588794268871567, 401.9948905765656377, 0.000000000000000000 ) ) ;
#15857 = DIRECTION ( 'NONE',  ( 0.000000000000000000, -0.000000000000000000, 1.000000000000000000 ) ) ;
#15858 = PRODUCT_DEFINITION ( 'UNKNOWN', '', #15588, #785 ) ;
#15859 = CARTESIAN_POINT ( 'NONE',  ( -24.70764059509555821, 369.1823905765655240, -19.99999999999999289 ) ) ;
#15860 = FACE_OUTER_BOUND ( 'NONE', #17203, .T. ) ;
#15861 = CARTESIAN_POINT ( 'NONE',  ( -10.20829729246300133, 486.3698905765655809, 7.653668647301790529 ) ) ;
#15862 = DIRECTION ( 'NONE',  ( 0.000000000000000000, -1.000000000000000000, 0.000000000000000000 ) ) ;
#15863 = CARTESIAN_POINT ( 'NONE',  ( -43.27177863848956463, 223.9102039777116033, 11.41195197239935233 ) ) ;
#15864 = CIRCLE ( 'NONE', #21023, 59.93977357075245038 ) ;
#15865 = CARTESIAN_POINT ( 'NONE',  ( -8.685887942688708563, 252.2448905601784475, -2.449293598294705724E-15 ) ) ;
#15866 = CARTESIAN_POINT ( 'NONE',  ( -10.20829729246298712, 366.3698905765655809, 7.653668647301790529 ) ) ;
#15867 = CARTESIAN_POINT ( 'NONE',  ( -35.09675569278795138, 433.4948905683720568, -15.47720386886985544 ) ) ;
#15868 = DIRECTION ( 'NONE',  ( 0.000000000000000000, 1.000000000000000000, -0.000000000000000000 ) ) ;
#15869 = CARTESIAN_POINT ( 'NONE',  ( -40.53162694259542320, 256.6198905683720568, 11.84573899990672885 ) ) ;
#15870 = EDGE_LOOP ( 'NONE', ( #18035, #19258, #6970, #5286, #13210, #4781 ) ) ;
#15871 = ORIENTED_EDGE ( 'NONE', *, *, #10107, .F. ) ;
#15872 = CARTESIAN_POINT ( 'NONE',  ( -28.68588794268872988, 479.4948905765656377, -19.99999999999999289 ) ) ;
#15873 = ORIENTED_EDGE ( 'NONE', *, *, #2238, .T. ) ;
#15874 = CARTESIAN_POINT ( 'NONE',  ( -32.01814843081345430, 473.1823905683720000, -16.75240474999999307 ) ) ;
#15875 = ORIENTED_EDGE ( 'NONE', *, *, #1041, .F. ) ;
#15876 = CARTESIAN_POINT ( 'NONE',  ( -14.54375231895776999, 363.4948905601784759, -14.14213562373094746 ) ) ;
#15877 = CARTESIAN_POINT ( 'NONE',  ( -32.01814843081343298, 231.6823905683720568, -16.75240474999999307 ) ) ;
#15878 = VERTEX_POINT ( 'NONE', #20931 ) ;
#15879 = CARTESIAN_POINT ( 'NONE',  ( -35.09675569278796559, 521.9948905683720568, -15.47720386886985544 ) ) ;
#15880 = DIRECTION ( 'NONE',  ( 0.000000000000000000, 0.000000000000000000, 1.000000000000000000 ) ) ;
#15881 = AXIS2_PLACEMENT_3D ( 'NONE', #10834, #5750, #1019 ) ;
#15882 = CARTESIAN_POINT ( 'NONE',  ( -40.01497788969915348, 470.4323905765656377, -16.95518130045146421 ) ) ;
#15883 = CARTESIAN_POINT ( 'NONE',  ( 0.2573354458087866448, -6.889406814520517841, 1.067197363239227759 ) ) ;
#15884 = FACE_OUTER_BOUND ( 'NONE', #21053, .T. ) ;
#15885 = LINE ( 'NONE', #15672, #6686 ) ;
#15886 = DIRECTION ( 'NONE',  ( 0.000000000000000000, 1.000000000000000000, -0.000000000000000000 ) ) ;
#15887 = FILL_AREA_STYLE_COLOUR ( '', #3189 ) ;
#15888 = CARTESIAN_POINT ( 'NONE',  ( -28.68588794268869790, 221.3698905683720284, -16.75240474999999307 ) ) ;
#15889 = CARTESIAN_POINT ( 'NONE',  ( -11.93348319268872260, 340.6823905683720000, -3.332260488124732856 ) ) ;
#15890 = DIRECTION ( 'NONE',  ( 0.000000000000000000, 0.000000000000000000, -1.000000000000000000 ) ) ;
#15891 = CARTESIAN_POINT ( 'NONE',  ( 4.700000000000000178, -7.505553499465150047, 0.000000000000000000 ) ) ;
#15892 = EDGE_CURVE ( 'NONE', #2298, #1002, #14133, .T. ) ;
#15893 = CARTESIAN_POINT ( 'NONE',  ( -11.93348319268872437, 388.5573905683720000, 3.332260488124728415 ) ) ;
#15894 = EDGE_CURVE ( 'NONE', #6826, #19261, #18891, .T. ) ;
#15895 = DIRECTION ( 'NONE',  ( 0.000000000000000000, -0.000000000000000000, 1.000000000000000000 ) ) ;
#15896 = CARTESIAN_POINT ( 'NONE',  ( -48.68588794268870856, 376.9323905601785327, -3.978247347593158345 ) ) ;
#15897 = CARTESIAN_POINT ( 'NONE',  ( -162.2727221670389781, 30.52886280891152282, -20.57735571454641033 ) ) ;
#15898 = VERTEX_POINT ( 'NONE', #10755 ) ;
#15899 = ORIENTED_EDGE ( 'NONE', *, *, #14792, .T. ) ;
#15900 = CARTESIAN_POINT ( 'NONE',  ( -19.19641293061499709, 508.8073905683720000, 14.20200298773971426 ) ) ;
#15901 = CARTESIAN_POINT ( 'NONE',  ( -64.27068722059112815, 585.7448905601785327, -35.12437985717895828 ) ) ;
#15902 = VERTEX_POINT ( 'NONE', #4491 ) ;
#15903 = CARTESIAN_POINT ( 'NONE',  ( -40.53162694259543031, 304.1198905683720000, -11.84573899990672707 ) ) ;
#15904 = VERTEX_POINT ( 'NONE', #20717 ) ;
#15905 = CARTESIAN_POINT ( 'NONE',  ( -42.88789093042842637, 322.9323905683720000, -9.489475012073736337 ) ) ;
#15906 = CARTESIAN_POINT ( 'NONE',  ( -28.68588794268870501, 259.4948905765655809, -19.99999999999999289 ) ) ;
#15907 = LINE ( 'NONE', #10805, #4818 ) ;
#15908 = CARTESIAN_POINT ( 'NONE',  ( -44.16309181155855867, 253.2448905683720284, -6.410867750099231266 ) ) ;
#15909 = CARTESIAN_POINT ( 'NONE',  ( -11.93348319268872437, 390.6823905683720568, -3.332260488124732856 ) ) ;
#15910 = EDGE_CURVE ( 'NONE', #19163, #10104, #8525, .T. ) ;
#15911 = LINE ( 'NONE', #8973, #10268 ) ;
#15912 = DIRECTION ( 'NONE',  ( 0.000000000000000000, 0.000000000000000000, 1.000000000000000000 ) ) ;
#15913 = CIRCLE ( 'NONE', #26, 10.00000000000000533 ) ;
#15914 = CARTESIAN_POINT ( 'NONE',  ( -48.68588794268867304, 511.6823905765656377, -3.978247347593264927 ) ) ;
#15915 = CARTESIAN_POINT ( 'NONE',  ( -14.48388495494900496, 437.9323905683720000, 9.489475012073732785 ) ) ;
#15916 = ORIENTED_EDGE ( 'NONE', *, *, #18023, .F. ) ;
#15917 = CARTESIAN_POINT ( 'NONE',  ( -14.54375231895778064, 443.4948905601784759, -14.14213562373094746 ) ) ;
#15918 = ORIENTED_EDGE ( 'NONE', *, *, #12797, .T. ) ;
#15919 = ORIENTED_EDGE ( 'NONE', *, *, #1555, .T. ) ;
#15920 = ORIENTED_EDGE ( 'NONE', *, *, #481, .T. ) ;
#15921 = CARTESIAN_POINT ( 'NONE',  ( 6.416697501590670427, 217.7548513357008630, -60.00000000000000000 ) ) ;
#15922 = CARTESIAN_POINT ( 'NONE',  ( -8.685887942688715668, 321.9323905601784759, 3.978247347593161010 ) ) ;
#15923 = EDGE_CURVE ( 'NONE', #16030, #5025, #19202, .T. ) ;
#15924 = CARTESIAN_POINT ( 'NONE',  ( -38.17536295476244845, 366.9323905683721136, 14.20200298773971781 ) ) ;
#15925 = AXIS2_PLACEMENT_3D ( 'NONE', #16731, #5452, #1918 ) ;
#15926 = DIRECTION ( 'NONE',  ( -1.191790137725560488E-16, 1.000000000000000000, -0.000000000000000000 ) ) ;
#15927 = AXIS2_PLACEMENT_3D ( 'NONE', #17974, #3175, #16378 ) ;
#15928 = CARTESIAN_POINT ( 'NONE',  ( -14.54375231895778420, 505.7448905765655809, 14.14213562373094568 ) ) ;
#15929 = CARTESIAN_POINT ( 'NONE',  ( -16.84014894278199037, 387.6198905683720568, 11.84573899990672530 ) ) ;
#15930 = CARTESIAN_POINT ( 'NONE',  ( -40.53162694259542320, 236.6198905683720284, 11.84573899990672885 ) ) ;
#15931 = AXIS2_PLACEMENT_3D ( 'NONE', #19504, #16166, #3179 ) ;
#15932 = CARTESIAN_POINT ( 'NONE',  ( -28.68588794268871922, 406.3698905683720000, 16.75240474999999307 ) ) ;
#15933 = CARTESIAN_POINT ( 'NONE',  ( -48.68588794268870856, 331.6823905765655809, -3.978247347593158345 ) ) ;
#15934 = CARTESIAN_POINT ( 'NONE',  ( -47.16347859291443712, 326.6198905601784759, -7.653668647301793193 ) ) ;
#15935 = CARTESIAN_POINT ( 'NONE',  ( -44.16309181155856578, 303.2448905683720000, -6.410867750099231266 ) ) ;
#15936 =( LENGTH_UNIT ( ) NAMED_UNIT ( * ) SI_UNIT ( .MILLI., .METRE. ) );
#15937 = CARTESIAN_POINT ( 'NONE',  ( -13.20868407381887089, 450.9948905683720000, -6.410867750099233042 ) ) ;
#15938 = ADVANCED_FACE ( 'NONE', ( #17684 ), #5891, .F. ) ;
#15939 = DIRECTION ( 'NONE',  ( -0.000000000000000000, -1.000000000000000000, -0.000000000000000000 ) ) ;
#15940 = LINE ( 'NONE', #6391, #10040 ) ;
#15941 = LINE ( 'NONE', #12687, #941 ) ;
#15942 = AXIS2_PLACEMENT_3D ( 'NONE', #17265, #10435, #12066 ) ;
#15943 = CARTESIAN_POINT ( 'NONE',  ( -45.43829269268870519, 365.0573905683720568, -3.332260488124726194 ) ) ;
#15944 = AXIS2_PLACEMENT_3D ( 'NONE', #8896, #3714, #12259 ) ;
#15945 = CARTESIAN_POINT ( 'NONE',  ( -38.17536295476246266, 495.4323905683720000, 14.20200298773971781 ) ) ;
#15946 =( REPRESENTATION_RELATIONSHIP ('NONE','NONE', #1888, #10694 ) REPRESENTATION_RELATIONSHIP_WITH_TRANSFORMATION ( #10831 )SHAPE_REPRESENTATION_RELATIONSHIP( ) );
#15947 = CARTESIAN_POINT ( 'NONE',  ( -47.16347859291445843, 497.8698905601784759, 7.653668647301805628 ) ) ;
#15948 = CARTESIAN_POINT ( 'NONE',  ( -13.20868407381885490, 319.4948905683720000, -6.410867750099233042 ) ) ;
#15949 = EDGE_LOOP ( 'NONE', ( #6586, #15802 ) ) ;
#15950 = DIRECTION ( 'NONE',  ( -0.000000000000000000, -0.000000000000000000, -1.000000000000000000 ) ) ;
#15951 = VERTEX_POINT ( 'NONE', #2552 ) ;
#15952 = CARTESIAN_POINT ( 'NONE',  ( -47.16347859291443712, 312.6198905765655809, 7.653668647301805628 ) ) ;
#15953 = CARTESIAN_POINT ( 'NONE',  ( -45.43829269268871940, 415.3698905683720568, 0.000000000000000000 ) ) ;
#15954 = CARTESIAN_POINT ( 'NONE',  ( -28.68588794268871567, 394.4948905765656377, 19.99999999999999289 ) ) ;
#15955 = DIRECTION ( 'NONE',  ( -0.000000000000000000, -0.000000000000000000, -1.000000000000000000 ) ) ;
#15956 = CARTESIAN_POINT ( 'NONE',  ( -13.20868407381887089, 449.4948905683720568, -6.410867750099233042 ) ) ;
#15957 = ORIENTED_EDGE ( 'NONE', *, *, #13008, .F. ) ;
#15958 = CARTESIAN_POINT ( 'NONE',  ( -45.43829269268872650, 463.5573905683720568, -3.332260488124726638 ) ) ;
#15959 = CARTESIAN_POINT ( 'NONE',  ( 154.7587007620219026, 620.7448905601785327, 10.81142786866622885 ) ) ;
#15960 = CARTESIAN_POINT ( 'NONE',  ( -8.685887942688726326, 396.9948905765656377, -2.449293598294705724E-15 ) ) ;
#15961 = LINE ( 'NONE', #7398, #6175 ) ;
#15962 =( GEOMETRIC_REPRESENTATION_CONTEXT ( 3 ) GLOBAL_UNCERTAINTY_ASSIGNED_CONTEXT ( ( #14829 ) ) GLOBAL_UNIT_ASSIGNED_CONTEXT ( ( #16111, #17721, #4953 ) ) REPRESENTATION_CONTEXT ( 'NONE', 'WORKASPACE' ) );
#15963 = CARTESIAN_POINT ( 'NONE',  ( -48.68588794268872277, 491.9948905765656377, 0.000000000000000000 ) ) ;
#15964 = CARTESIAN_POINT ( 'NONE',  ( 2.112500170452225440E-15, -5.309483803148807191, -3.803704290982254932 ) ) ;
#15965 = CARTESIAN_POINT ( 'NONE',  ( 164.2593879927715932, 166.6963511708817691, -60.00000000000000000 ) ) ;
#15966 = CARTESIAN_POINT ( 'NONE',  ( 78.68120802659203150, 149.7457237375499517, 66.14548919766383506 ) ) ;
#15967 = DIRECTION ( 'NONE',  ( 0.000000000000000000, 1.000000000000000000, -0.000000000000000000 ) ) ;
#15968 = CARTESIAN_POINT ( 'NONE',  ( -38.53300430798842058, 223.9102039777116602, 16.90666462915203638 ) ) ;
#15969 = ADVANCED_FACE ( 'NONE', ( #6100 ), #19095, .F. ) ;
#15970 =( BOUNDED_CURVE ( )  B_SPLINE_CURVE ( 2, ( #7960, #1936, #13287, #6667, #16530, #1715, #18353, #19872, #15227, #11964, #5263, #420, #11649, #3435, #8282, #9909, #6986 ),
 .UNSPECIFIED., .F., .T. ) 
 B_SPLINE_CURVE_WITH_KNOTS ( ( 3, 2, 2, 2, 2, 2, 2, 2, 3 ),
 ( 0.3593750000000001110, 0.3613281250000001110, 0.3632812500000001110, 0.3652343750000001110, 0.3671875000000001110, 0.3691406250000001665, 0.3710937500000001665, 0.3730468750000001665, 0.3750000000000001665 ),
 .UNSPECIFIED. ) 
 CURVE ( )  GEOMETRIC_REPRESENTATION_ITEM ( )  RATIONAL_B_SPLINE_CURVE ( ( 0.9999999999999988898, 0.9807852804032315408, 1.000000000000000000, 0.9807852804032304306, 1.000000000000000000, 0.9807852804032304306, 1.000000000000000000, 0.9807852804032304306, 1.000000000000000000, 0.9807852804032304306, 1.000000000000000000, 0.9807852804032304306, 1.000000000000000000, 0.9807852804032304306, 1.000000000000000000, 0.9807852804032287652, 1.000000000000001554 ) ) 
 REPRESENTATION_ITEM ( '' )  );
#15971 = EDGE_CURVE ( 'NONE', #1814, #12774, #1627, .T. ) ;
#15972 = CARTESIAN_POINT ( 'NONE',  ( -11.73070664223723192, 241.3073905601784759, 11.32908994701042005 ) ) ;
#15973 = DIRECTION ( 'NONE',  ( 1.000000000000000000, 0.000000000000000000, 0.000000000000000000 ) ) ;
#15974 = CARTESIAN_POINT ( 'NONE',  ( -22.27502019258949417, 422.2448905683720568, -15.47720386886985544 ) ) ;
#15975 = CARTESIAN_POINT ( 'NONE',  ( -47.16347859291444422, 386.6198905601784759, -7.653668647301793193 ) ) ;
#15976 = CARTESIAN_POINT ( 'NONE',  ( -44.16309181155855157, 255.9948905683720568, 6.410867750099241924 ) ) ;
#15977 = VERTEX_POINT ( 'NONE', #7826 ) ;
#15978 = ORIENTED_EDGE ( 'NONE', *, *, #19227, .F. ) ;
#15979 = CARTESIAN_POINT ( 'NONE',  ( -21.03221929538693757, 478.8698905765656377, -18.47759065022572855 ) ) ;
#15980 = ORIENTED_EDGE ( 'NONE', *, *, #15503, .F. ) ;
#15981 = CARTESIAN_POINT ( 'NONE',  ( -40.53162694259545162, 464.1198905683720568, -11.84573899990672707 ) ) ;
#15982 = CARTESIAN_POINT ( 'NONE',  ( -42.82802356641964536, 230.7448905765656093, -14.14213562373094746 ) ) ;
#15983 = EDGE_CURVE ( 'NONE', #2560, #15706, #266, .T. ) ;
#15984 = VERTEX_POINT ( 'NONE', #2874 ) ;
#15985 = CARTESIAN_POINT ( 'NONE',  ( -8.685887942689042518, 526.6823905765655809, 3.978247347593879546 ) ) ;
#15986 = CARTESIAN_POINT ( 'NONE',  ( -45.43829269268869808, 233.8698905683720284, 0.000000000000000000 ) ) ;
#15987 = EDGE_CURVE ( 'NONE', #6213, #4291, #14456, .T. ) ;
#15988 = ORIENTED_EDGE ( 'NONE', *, *, #5192, .F. ) ;
#15989 = CARTESIAN_POINT ( 'NONE',  ( -40.53162694259545873, 532.6198905683720568, -11.84573899990672707 ) ) ;
#15990 = LINE ( 'NONE', #7312, #9359 ) ;
#15991 = ADVANCED_FACE ( 'NONE', ( #9769 ), #11617, .F. ) ;
#15992 = CARTESIAN_POINT ( 'NONE',  ( -8.685887942688735208, 457.3073905765655809, -3.978247347593165895 ) ) ;
#15993 = PRODUCT ( 'Coarse Pitch Steep Screw Shaft', 'Coarse Pitch Steep Screw Shaft', '', ( #8676 ) ) ;
#15994 = CARTESIAN_POINT ( 'NONE',  ( -40.01497788969913216, 348.8073905601784759, 16.95518130045146776 ) ) ;
#15995 = FILL_AREA_STYLE_COLOUR ( '', #10807 ) ;
#15996 = CARTESIAN_POINT ( 'NONE',  ( -24.70764059509554755, 239.1823905765656093, -19.99999999999999289 ) ) ;
#15997 = LINE ( 'NONE', #2470, #1530 ) ;
#15998 = CARTESIAN_POINT ( 'NONE',  ( -10.23462588383483762, 223.9102039777117454, 7.884011575492554158 ) ) ;
#15999 = CARTESIAN_POINT ( 'NONE',  ( -35.09675569278793716, 225.7448905683720568, 15.47720386886985366 ) ) ;
#16000 = CARTESIAN_POINT ( 'NONE',  ( -19.19641293061497933, 318.8073905683720568, 14.20200298773971426 ) ) ;
#16001 = ADVANCED_FACE ( 'NONE', ( #8038 ), #11290, .F. ) ;
#16002 = CARTESIAN_POINT ( 'NONE',  ( -32.66413529028185536, 235.0573905601785043, -19.99999999999999289 ) ) ;
#16003 = DIRECTION ( 'NONE',  ( 0.000000000000000000, 0.000000000000000000, 1.000000000000000000 ) ) ;
#16004 = CARTESIAN_POINT ( 'NONE',  ( -38.17536295476244845, 313.8073905683720000, -14.20200298773971426 ) ) ;
#16005 = CARTESIAN_POINT ( 'NONE',  ( -28.68588794268871922, 381.3698905683720568, -16.75240474999999307 ) ) ;
#16006 = CARTESIAN_POINT ( 'NONE',  ( -32.01814843081346140, 527.5573905683720568, 16.75240474999999307 ) ) ;
#16007 = CIRCLE ( 'NONE', #6318, 4.000000000000001776 ) ;
#16008 = CARTESIAN_POINT ( 'NONE',  ( -36.33955658999050797, 385.3698905601785327, -18.47759065022572855 ) ) ;
#16009 = CARTESIAN_POINT ( 'NONE',  ( -48.68588794268869435, 231.9948905765656377, 0.000000000000000000 ) ) ;
#16010 = EDGE_LOOP ( 'NONE', ( #5905, #2060, #18778, #15389 ) ) ;
#16011 = ORIENTED_EDGE ( 'NONE', *, *, #3922, .F. ) ;
#16012 = CARTESIAN_POINT ( 'NONE',  ( -44.16309181155858710, 494.7448905683720000, -6.410867750099231266 ) ) ;
#16013 = FACE_OUTER_BOUND ( 'NONE', #402, .T. ) ;
#16014 = ORIENTED_EDGE ( 'NONE', *, *, #4938, .T. ) ;
#16015 = CARTESIAN_POINT ( 'NONE',  ( -35.09675569278794427, 307.2448905683720000, 15.47720386886985366 ) ) ;
#16016 = CARTESIAN_POINT ( 'NONE',  ( -22.27502019258948351, 320.7448905683720000, -15.47720386886985544 ) ) ;
#16017 = AXIS2_PLACEMENT_3D ( 'NONE', #17408, #4092, #10573 ) ;
#16018 = CARTESIAN_POINT ( 'NONE',  ( -24.70764059509553690, 264.8073905765656377, 19.99999999999998934 ) ) ;
#16019 = FACE_OUTER_BOUND ( 'NONE', #8956, .T. ) ;
#16020 = CARTESIAN_POINT ( 'NONE',  ( -28.68588794268875120, 610.7448905601785327, 0.000000000000000000 ) ) ;
#16021 = VECTOR ( 'NONE', #15119, 1000.000000000000000 ) ;
#16022 = CARTESIAN_POINT ( 'NONE',  ( -19.19641293061498644, 388.8073905683720568, 14.20200298773971426 ) ) ;
#16023 = CARTESIAN_POINT ( 'NONE',  ( -11.73070664223724613, 333.1823905601784190, -11.32908994701042538 ) ) ;
#16024 = CARTESIAN_POINT ( 'NONE',  ( 5.299999999999999822, 3.752776749732560368, -6.499999999999999112 ) ) ;
#16025 = CARTESIAN_POINT ( 'NONE',  ( -8.685887942688617969, 242.5573905601784759, -3.978247347592952732 ) ) ;
#16026 = CARTESIAN_POINT ( 'NONE',  ( -38.17536295476246266, 442.3073905683721136, -14.20200298773971426 ) ) ;
#16027 = DIRECTION ( 'NONE',  ( -0.000000000000000000, -0.000000000000000000, -1.000000000000000000 ) ) ;
#16028 = ORIENTED_EDGE ( 'NONE', *, *, #4938, .F. ) ;
#16029 = CARTESIAN_POINT ( 'NONE',  ( -48.68588794268871567, 446.9323905601784759, -3.978247347593158345 ) ) ;
#16030 = VERTEX_POINT ( 'NONE', #19516 ) ;
#16031 = EDGE_LOOP ( 'NONE', ( #6141, #16967, #12346 ) ) ;
#16032 = ORIENTED_EDGE ( 'NONE', *, *, #8818, .T. ) ;
#16033 = CARTESIAN_POINT ( 'NONE',  ( 158.8141120573112630, 610.7448905601785327, 0.000000000000000000 ) ) ;
#16034 = CARTESIAN_POINT ( 'NONE',  ( -17.35679799567828852, 320.6823905601784759, 16.95518130045146421 ) ) ;
#16035 = LINE ( 'NONE', #17748, #20372 ) ;
#16036 = VECTOR ( 'NONE', #15809, 1000.000000000000000 ) ;
#16037 = CIRCLE ( 'NONE', #6687, 6.500000000000000888 ) ;
#16038 = EDGE_CURVE ( 'NONE', #880, #12697, #1904, .T. ) ;
#16039 = CARTESIAN_POINT ( 'NONE',  ( -44.16309181155857289, 354.7448905683720568, -6.410867750099231266 ) ) ;
#16040 = DIRECTION ( 'NONE',  ( 1.000000000000000000, 0.000000000000000000, 0.000000000000000000 ) ) ;
#16041 = CARTESIAN_POINT ( 'NONE',  ( -40.01497788969915348, 500.4323905765656946, -16.95518130045146421 ) ) ;
#16042 = CARTESIAN_POINT ( 'NONE',  ( -11.93348319268872260, 378.8698905683720000, -2.051577885510841163E-15 ) ) ;
#16043 = CARTESIAN_POINT ( 'NONE',  ( -32.66413529028186247, 309.8073905765656377, -19.99999999999999289 ) ) ;
#16044 = CARTESIAN_POINT ( 'NONE',  ( -40.53162694259544452, 412.6198905683720568, -11.84573899990672707 ) ) ;
#16045 = CARTESIAN_POINT ( 'NONE',  ( -8.685887942688719221, 326.9948905765656377, -2.449293598294705724E-15 ) ) ;
#16046 = DIRECTION ( 'NONE',  ( 1.000000000000000000, 0.000000000000000000, 0.000000000000000000 ) ) ;
#16047 = CARTESIAN_POINT ( 'NONE',  ( -13.20868407381885312, 299.4948905683720568, -6.410867750099233042 ) ) ;
#16048 = CARTESIAN_POINT ( 'NONE',  ( -14.48388495494900674, 449.4323905683720568, 9.489475012073732785 ) ) ;
#16049 = FACE_OUTER_BOUND ( 'NONE', #14859, .T. ) ;
#16050 = DIRECTION ( 'NONE',  ( -0.000000000000000000, -0.000000000000000000, 1.000000000000000000 ) ) ;
#16051 = DIRECTION ( 'NONE',  ( -1.000000000000000000, 0.000000000000000000, 0.000000000000000000 ) ) ;
#16052 = EDGE_CURVE ( 'NONE', #8775, #20838, #16395, .T. ) ;
#16053 = CARTESIAN_POINT ( 'NONE',  ( -16.84014894278199037, 371.6198905683720000, -11.84573899990672707 ) ) ;
#16054 = CARTESIAN_POINT ( 'NONE',  ( -11.93348319268873858, 498.8698905683720000, -2.051577885510841163E-15 ) ) ;
#16055 = CARTESIAN_POINT ( 'NONE',  ( -48.68588794268872277, 507.2448905601785327, 0.000000000000000000 ) ) ;
#16056 = CARTESIAN_POINT ( 'NONE',  ( -40.53162694259543031, 315.1198905683720568, 11.84573899990672885 ) ) ;
#16057 = ORIENTED_EDGE ( 'NONE', *, *, #4665, .F. ) ;
#16058 = CARTESIAN_POINT ( 'NONE',  ( -14.54375231895775400, 260.9948905601784759, 14.14213562373094568 ) ) ;
#16059 = ORIENTED_EDGE ( 'NONE', *, *, #5592, .T. ) ;
#16060 = DIRECTION ( 'NONE',  ( 1.191790137725560488E-16, -1.000000000000000000, -0.000000000000000000 ) ) ;
#16061 = ADVANCED_FACE ( 'NONE', ( #21249 ), #16716, .F. ) ;
#16062 = CARTESIAN_POINT ( 'NONE',  ( -16.84014894278199748, 431.6198905683720000, -11.84573899990672707 ) ) ;
#16063 = DIRECTION ( 'NONE',  ( 0.000000000000000000, 0.000000000000000000, 1.000000000000000000 ) ) ;
#16064 = CYLINDRICAL_SURFACE ( 'NONE', #11075, 20.00000000000000000 ) ;
#16065 = CARTESIAN_POINT ( 'NONE',  ( -45.43829269268871940, 443.8698905683720568, 0.000000000000000000 ) ) ;
#16066 = ORIENTED_EDGE ( 'NONE', *, *, #17134, .F. ) ;
#16067 = CARTESIAN_POINT ( 'NONE',  ( -28.68588794268872277, 456.3698905683720000, 16.75240474999999307 ) ) ;
#16068 = CARTESIAN_POINT ( 'NONE',  ( -14.54375231895777532, 413.4948905601784759, -14.14213562373094746 ) ) ;
#16069 = CARTESIAN_POINT ( 'NONE',  ( -17.35679799567830273, 388.5573905765656377, -16.95518130045146421 ) ) ;
#16070 = CARTESIAN_POINT ( 'NONE',  ( -42.82802356641965957, 370.7448905765656377, -14.14213562373094746 ) ) ;
#16071 = CARTESIAN_POINT ( 'NONE',  ( 0.5805565836007642311, -3.752776749732576356, -6.499999999999999112 ) ) ;
#16072 = CARTESIAN_POINT ( 'NONE',  ( 51.98467606588575052, 30.52886280891152282, -117.7257097687431298 ) ) ;
#16073 = CARTESIAN_POINT ( 'NONE',  ( -28.68588794268874054, 600.7448905601785327, 20.00000000000000355 ) ) ;
#16074 =( REPRESENTATION_RELATIONSHIP ('NONE','NONE', #1888, #21199 ) REPRESENTATION_RELATIONSHIP_WITH_TRANSFORMATION ( #13244 )SHAPE_REPRESENTATION_RELATIONSHIP( ) );
#16075 = CARTESIAN_POINT ( 'NONE',  ( -11.93348319268872793, 420.6823905683720000, -3.332260488124732856 ) ) ;
#16076 = DIRECTION ( 'NONE',  ( 0.8090169943749473402, 0.000000000000000000, -0.5877852522924732481 ) ) ;
#16077 = CARTESIAN_POINT ( 'NONE',  ( -40.53162694259542320, 254.1198905683720284, -11.84573899990672707 ) ) ;
#16078 = EDGE_LOOP ( 'NONE', ( #656, #4808, #15581, #17221, #12727, #12020, #13234 ) ) ;
#16079 = ORIENTED_EDGE ( 'NONE', *, *, #19266, .T. ) ;
#16080 = CARTESIAN_POINT ( 'NONE',  ( -10.20829729246299422, 426.3698905765656377, 7.653668647301790529 ) ) ;
#16081 = VERTEX_POINT ( 'NONE', #16288 ) ;
#16082 = CARTESIAN_POINT ( 'NONE',  ( -28.68588794268872988, 472.8698905683720568, -16.75240474999999307 ) ) ;
#16083 = CARTESIAN_POINT ( 'NONE',  ( -47.16347859291443001, 231.3698905765656093, -7.653668647301793193 ) ) ;
#16084 = EDGE_LOOP ( 'NONE', ( #15606, #14091, #18914, #18508 ) ) ;
#16085 = CARTESIAN_POINT ( 'NONE',  ( -47.16347859291446554, 522.6198905765655809, 7.653668647301805628 ) ) ;
#16086 = CARTESIAN_POINT ( 'NONE',  ( -11.93348319268870661, 228.5573905683720568, 3.332260488124728415 ) ) ;
#16087 = VERTEX_POINT ( 'NONE', #14670 ) ;
#16088 = CARTESIAN_POINT ( 'NONE',  ( -19.19641293061500420, 530.4323905683720568, -14.20200298773971603 ) ) ;
#16089 = CARTESIAN_POINT ( 'NONE',  ( 72.94945500224395118, 285.0140030772282103, 20.00000000000000355 ) ) ;
#16090 = CARTESIAN_POINT ( 'NONE',  ( -28.68588794268872277, 434.4948905765655809, 19.99999999999999289 ) ) ;
#16091 = CYLINDRICAL_SURFACE ( 'NONE', #2373, 50.00000000000000000 ) ;
#16092 = CARTESIAN_POINT ( 'NONE',  ( 10.41669750159067220, 217.7548513357008630, -49.99999999999999289 ) ) ;
#16093 = CARTESIAN_POINT ( 'NONE',  ( 158.8141120573112630, 575.7448905601785327, 10.00000000000000888 ) ) ;
#16094 = CARTESIAN_POINT ( 'NONE',  ( -32.66413529028186247, 289.4323905601784190, 19.99999999999999289 ) ) ;
#16095 =( BOUNDED_CURVE ( )  B_SPLINE_CURVE ( 2, ( #7634, #10659, #2356, #12518, #20735, #14368, #17591, #12298, #17277, #14148, #10769, #2567, #15876, #2463, #2783, #15769, #9371 ),
 .UNSPECIFIED., .F., .T. ) 
 B_SPLINE_CURVE_WITH_KNOTS ( ( 3, 2, 2, 2, 2, 2, 2, 2, 3 ),
 ( 0.5312500000000003331, 0.5332031250000003331, 0.5351562500000003331, 0.5371093750000003331, 0.5390625000000003331, 0.5410156250000003331, 0.5429687500000003331, 0.5449218750000003331, 0.5468750000000003331 ),
 .UNSPECIFIED. ) 
 CURVE ( )  GEOMETRIC_REPRESENTATION_ITEM ( )  RATIONAL_B_SPLINE_CURVE ( ( 0.9999999999999966693, 0.9807852804032337612, 1.000000000000000000, 0.9807852804032304306, 1.000000000000000000, 0.9807852804032304306, 1.000000000000000000, 0.9807852804032304306, 1.000000000000000000, 0.9807852804032304306, 1.000000000000000000, 0.9807852804032304306, 1.000000000000000000, 0.9807852804032304306, 1.000000000000000000, 0.9807852804032270999, 1.000000000000003331 ) ) 
 REPRESENTATION_ITEM ( '' )  );
#16096 =( LENGTH_UNIT ( ) NAMED_UNIT ( * ) SI_UNIT ( .MILLI., .METRE. ) );
#16097 = CARTESIAN_POINT ( 'NONE',  ( -25.35362745456397349, 221.0573905683720284, -16.75240474999999307 ) ) ;
#16098 = CARTESIAN_POINT ( 'NONE',  ( -32.01814843081344009, 313.1823905683720000, -16.75240474999999307 ) ) ;
#16099 = EDGE_CURVE ( 'NONE', #12049, #4779, #13014, .T. ) ;
#16100 = CARTESIAN_POINT ( 'NONE',  ( 6.416697501590670427, 172.9933428177121471, 45.00000000000000000 ) ) ;
#16101 = CARTESIAN_POINT ( 'NONE',  ( 20.60949999999999349, 0.000000000000000000, 4.000000000000000000 ) ) ;
#16102 = EDGE_CURVE ( 'NONE', #12697, #7658, #18318, .T. ) ;
#16103 = CARTESIAN_POINT ( 'NONE',  ( -35.09675569278793716, 303.4948905683720568, -15.47720386886985544 ) ) ;
#16104 = EDGE_CURVE ( 'NONE', #2702, #604, #11508, .T. ) ;
#16105 = CARTESIAN_POINT ( 'NONE',  ( -44.16309181155856578, 374.4948905683720000, 6.410867750099241924 ) ) ;
#16106 = CARTESIAN_POINT ( 'NONE',  ( -13.20868407381888154, 530.9948905683720568, -6.410867750099233042 ) ) ;
#16107 = CARTESIAN_POINT ( 'NONE',  ( -21.03221929538690915, 370.3698905601784759, 18.47759065022572500 ) ) ;
#16108 = DIRECTION ( 'NONE',  ( -0.000000000000000000, 0.5000000000000011102, 0.8660254037844379305 ) ) ;
#16109 = VERTEX_POINT ( 'NONE', #5126 ) ;
#16110 = CARTESIAN_POINT ( 'NONE',  ( -32.01814843081346140, 483.1823905683720000, -16.75240474999999307 ) ) ;
#16111 =( LENGTH_UNIT ( ) NAMED_UNIT ( * ) SI_UNIT ( .MILLI., .METRE. ) );
#16112 = CARTESIAN_POINT ( 'NONE',  ( -11.93348319268871371, 289.1823905683720000, -3.332260488124732856 ) ) ;
#16113 = ORIENTED_EDGE ( 'NONE', *, *, #17082, .F. ) ;
#16114 = EDGE_CURVE ( 'NONE', #12838, #13843, #7131, .T. ) ;
#16115 = CARTESIAN_POINT ( 'NONE',  ( -11.93348319268871194, 290.6823905683720568, -3.332260488124732856 ) ) ;
#16116 = CARTESIAN_POINT ( 'NONE',  ( -28.68588794268870856, 326.3698905683720000, 16.75240474999999307 ) ) ;
#16117 = CARTESIAN_POINT ( 'NONE',  ( -14.48388495494898542, 259.4323905683720568, 9.489475012073731008 ) ) ;
#16118 = CARTESIAN_POINT ( 'NONE',  ( -47.16347859291443001, 261.3698905765656377, -7.653668647301793193 ) ) ;
#16119 = DIRECTION ( 'NONE',  ( -1.191790137725560488E-16, 1.000000000000000000, -0.000000000000000000 ) ) ;
#16120 = LINE ( 'NONE', #1846, #18563 ) ;
#16121 = CARTESIAN_POINT ( 'NONE',  ( -40.53162694259543741, 374.1198905683720000, -11.84573899990672707 ) ) ;
#16122 = CIRCLE ( 'NONE', #18868, 49.93977357075243617 ) ;
#16123 = PLANE ( 'NONE',  #2340 ) ;
#16124 = CARTESIAN_POINT ( 'NONE',  ( 20.74841189052421697, 600.7448905601785327, -7.500000000000000000 ) ) ;
#16125 = DIRECTION ( 'NONE',  ( 0.000000000000000000, 0.000000000000000000, 1.000000000000000000 ) ) ;
#16126 = AXIS2_PLACEMENT_3D ( 'NONE', #19231, #17499, #10892 ) ;
#16127 = CARTESIAN_POINT ( 'NONE',  ( -16.84014894278200103, 450.1198905683720568, -11.84573899990672707 ) ) ;
#16128 = CARTESIAN_POINT ( 'NONE',  ( 30.42502041961814996, 180.1716627696692967, -40.00000000000000000 ) ) ;
#16129 = EDGE_LOOP ( 'NONE', ( #13692, #1774, #18755, #1854 ) ) ;
#16130 = CARTESIAN_POINT ( 'NONE',  ( -11.73070664223725856, 433.1823905601785327, -11.32908994701042715 ) ) ;
#16131 = VERTEX_POINT ( 'NONE', #3300 ) ;
#16132 = ORIENTED_EDGE ( 'NONE', *, *, #8147, .F. ) ;
#16133 = ORIENTED_EDGE ( 'NONE', *, *, #5051, .T. ) ;
#16134 = CARTESIAN_POINT ( 'NONE',  ( -43.68588794268869435, 210.1437886375728965, -2.161864096862809871E-19 ) ) ;
#16135 = CARTESIAN_POINT ( 'NONE',  ( -48.68588794268870146, 326.9323905601784759, -3.978247347593158345 ) ) ;
#16136 = CARTESIAN_POINT ( 'NONE',  ( -46.31968306282883674, 213.9102039777116602, 33.59072564020503648 ) ) ;
#16137 = CARTESIAN_POINT ( 'NONE',  ( -16.84014894278199037, 351.6198905683720000, -11.84573899990672707 ) ) ;
#16138 = VECTOR ( 'NONE', #14885, 1000.000000000000000 ) ;
#16139 = CARTESIAN_POINT ( 'NONE',  ( -8.685887942688735208, 585.7448905601785327, 0.000000000000000000 ) ) ;
#16140 = CARTESIAN_POINT ( 'NONE',  ( -36.33955658999053639, 503.8698905765656377, 18.47759065022572500 ) ) ;
#16141 = CARTESIAN_POINT ( 'NONE',  ( -35.09675569278795138, 391.9948905683720568, -15.47720386886985544 ) ) ;
#16142 = CARTESIAN_POINT ( 'NONE',  ( -38.17536295476244135, 223.8073905683720284, -14.20200298773971426 ) ) ;
#16143 = CARTESIAN_POINT ( 'NONE',  ( -44.16309181155856578, 384.4948905683720000, 6.410867750099241924 ) ) ;
#16144 = CIRCLE ( 'NONE', #6796, 4.000000000000001776 ) ;
#16145 = CARTESIAN_POINT ( 'NONE',  ( -48.68588794268870856, 331.9948905765656377, 0.000000000000000000 ) ) ;
#16146 = CARTESIAN_POINT ( 'NONE',  ( -8.685887942688641061, 422.5573905601784759, -3.978247347592952732 ) ) ;
#16147 = CARTESIAN_POINT ( 'NONE',  ( -14.48388495494898720, 277.9323905683720568, 9.489475012073731008 ) ) ;
#16148 = CARTESIAN_POINT ( 'NONE',  ( -38.17536295476245556, 446.9323905683720000, 14.20200298773971781 ) ) ;
#16149 = CARTESIAN_POINT ( 'NONE',  ( -8.685887942688536256, 282.5573905601784190, -3.978247347592740013 ) ) ;
#16150 = CARTESIAN_POINT ( 'NONE',  ( -36.33955658999051508, 369.1198905601785327, 18.47759065022572500 ) ) ;
#16151 = DIRECTION ( 'NONE',  ( -1.191790137725560488E-16, 1.000000000000000000, -0.000000000000000000 ) ) ;
#16152 = EDGE_CURVE ( 'NONE', #11679, #20997, #20275, .T. ) ;
#16153 = AXIS2_PLACEMENT_3D ( 'NONE', #3400, #19944, #19724 ) ;
#16154 = CARTESIAN_POINT ( 'NONE',  ( -42.88789093042843348, 346.3073905683720568, 9.489475012073736337 ) ) ;
#16155 = CARTESIAN_POINT ( 'NONE',  ( -44.16309181155858710, 493.2448905683720000, -6.410867750099231266 ) ) ;
#16156 = CARTESIAN_POINT ( 'NONE',  ( -28.68588794268873343, 504.7448905601785896, -19.99999999999999289 ) ) ;
#16157 = CARTESIAN_POINT ( 'NONE',  ( -11.93348319268871549, 318.8698905683720000, -2.051577885510841163E-15 ) ) ;
#16158 = AXIS2_PLACEMENT_3D ( 'NONE', #16363, #19592, #4771 ) ;
#16159 = EDGE_LOOP ( 'NONE', ( #1778, #3016, #18807, #13317 ) ) ;
#16160 = CARTESIAN_POINT ( 'NONE',  ( -8.685887942688422569, 522.5573905601784190, -3.978247347592394068 ) ) ;
#16161 = VERTEX_POINT ( 'NONE', #14770 ) ;
#16162 = LINE ( 'NONE', #1553, #7396 ) ;
#16163 = EDGE_CURVE ( 'NONE', #11848, #9040, #14880, .T. ) ;
#16164 = CARTESIAN_POINT ( 'NONE',  ( 146.3141120573112630, 610.7448905601785327, 0.000000000000000000 ) ) ;
#16165 = CARTESIAN_POINT ( 'NONE',  ( -28.68588794268871922, 427.8698905683720568, 16.75240474999999307 ) ) ;
#16166 = DIRECTION ( 'NONE',  ( -1.000000000000000000, -0.000000000000000000, -0.000000000000000000 ) ) ;
#16167 = DIRECTION ( 'NONE',  ( -0.000000000000000000, -0.000000000000000000, 1.000000000000000000 ) ) ;
#16168 = CARTESIAN_POINT ( 'NONE',  ( -38.17536295476245556, 445.4323905683720568, 14.20200298773971781 ) ) ;
#16169 = ORIENTED_EDGE ( 'NONE', *, *, #21038, .T. ) ;
#16170 = CARTESIAN_POINT ( 'NONE',  ( -35.09675569278796559, 455.7448905683720568, 15.47720386886985366 ) ) ;
#16171 = DIRECTION ( 'NONE',  ( -3.836511174089486666E-16, 0.000000000000000000, -1.000000000000000000 ) ) ;
#16172 = CARTESIAN_POINT ( 'NONE',  ( -36.33955658999050797, 380.1198905765656377, -18.47759065022572855 ) ) ;
#16173 = DIRECTION ( 'NONE',  ( -1.191790137725560488E-16, 1.000000000000000000, -0.000000000000000000 ) ) ;
#16174 = CARTESIAN_POINT ( 'NONE',  ( -28.68588794268875120, 585.7448905601785327, 0.000000000000000000 ) ) ;
#16175 = CARTESIAN_POINT ( 'NONE',  ( -11.73070664223725856, 427.9323905765656377, -11.32908994701042538 ) ) ;
#16176 = CARTESIAN_POINT ( 'NONE',  ( -28.68588794268869790, 254.4948905765656093, 19.99999999999999289 ) ) ;
#16177 = CARTESIAN_POINT ( 'NONE',  ( -14.48388495494901740, 519.4323905683720568, 9.489475012073732785 ) ) ;
#16178 = DIRECTION ( 'NONE',  ( -0.000000000000000000, 1.000000000000000000, 0.000000000000000000 ) ) ;
#16179 = CYLINDRICAL_SURFACE ( 'NONE', #9398, 15.00000000000000355 ) ;
#16180 = CARTESIAN_POINT ( 'NONE',  ( -8.685887942688720997, 342.2448905601784759, -2.449293598294705724E-15 ) ) ;
#16181 = EDGE_CURVE ( 'NONE', #10452, #7286, #6522, .T. ) ;
#16182 = CARTESIAN_POINT ( 'NONE',  ( -44.16309181155857999, 434.7448905683720000, -6.410867750099231266 ) ) ;
#16183 = CARTESIAN_POINT ( 'NONE',  ( -10.20829729246297646, 266.3698905765656377, 7.653668647301790529 ) ) ;
#16184 = CARTESIAN_POINT ( 'NONE',  ( -35.09675569278793006, 253.4948905683720568, -15.47720386886985544 ) ) ;
#16185 = ORIENTED_EDGE ( 'NONE', *, *, #12661, .F. ) ;
#16186 = ORIENTED_EDGE ( 'NONE', *, *, #5592, .F. ) ;
#16187 = CARTESIAN_POINT ( 'NONE',  ( -28.68588794268869435, 188.9102039777116602, 0.000000000000000000 ) ) ;
#16188 = ORIENTED_EDGE ( 'NONE', *, *, #10326, .T. ) ;
#16189 = CARTESIAN_POINT ( 'NONE',  ( -25.35362745456400546, 472.5573905683720568, -16.75240474999999307 ) ) ;
#16190 = CARTESIAN_POINT ( 'NONE',  ( -21.03221929538690560, 218.8698905765656377, -18.47759065022572855 ) ) ;
#16191 = ORIENTED_EDGE ( 'NONE', *, *, #9621, .T. ) ;
#16192 = DIRECTION ( 'NONE',  ( 1.000000000000000000, 0.000000000000000000, 0.000000000000000000 ) ) ;
#16193 = CARTESIAN_POINT ( 'NONE',  ( -11.93348319268874214, 530.6823905683721705, -3.332260488124732856 ) ) ;
#16194 = ORIENTED_EDGE ( 'NONE', *, *, #20462, .T. ) ;
#16195 = CARTESIAN_POINT ( 'NONE',  ( -32.01814843081346140, 526.0573905683720568, 16.75240474999999307 ) ) ;
#16196 = CARTESIAN_POINT ( 'NONE',  ( -123.2946569474810303, 30.52886280891152282, -20.57735571454641388 ) ) ;
#16197 = ADVANCED_FACE ( 'NONE', ( #6632 ), #19729, .T. ) ;
#16198 = CARTESIAN_POINT ( 'NONE',  ( -45.64106924314019409, 441.0573905765656377, -11.32908994701042715 ) ) ;
#16199 = DIRECTION ( 'NONE',  ( 0.000000000000000000, 1.000000000000000000, 0.000000000000000000 ) ) ;
#16200 = CARTESIAN_POINT ( 'NONE',  ( -25.35362745456399125, 351.0573905683720000, -16.75240474999999307 ) ) ;
#16201 = DIRECTION ( 'NONE',  ( 0.000000000000000000, 0.000000000000000000, -1.000000000000000000 ) ) ;
#16202 = CARTESIAN_POINT ( 'NONE',  ( -8.685887942688742314, 573.2448905601785327, 2.449293598294706119E-15 ) ) ;
#16203 = CARTESIAN_POINT ( 'NONE',  ( -48.68588794268872277, 507.2448905601785327, 0.000000000000000000 ) ) ;
#16204 = AXIS2_PLACEMENT_3D ( 'NONE', #18111, #6324, #3307 ) ;
#16205 = DIRECTION ( 'NONE',  ( 1.000000000000000000, 0.000000000000000000, 0.000000000000000000 ) ) ;
#16206 = CARTESIAN_POINT ( 'NONE',  ( -28.68588794268869435, 226.3698905683720284, 16.75240474999999307 ) ) ;
#16207 = CARTESIAN_POINT ( 'NONE',  ( -44.16309181155856578, 314.7448905683720000, -6.410867750099231266 ) ) ;
#16208 = EDGE_CURVE ( 'NONE', #9825, #4497, #13254, .T. ) ;
#16209 = CARTESIAN_POINT ( 'NONE',  ( -24.70764059509556887, 444.4323905601784759, -19.99999999999999289 ) ) ;
#16210 = DIRECTION ( 'NONE',  ( 0.000000000000000000, 1.000000000000000000, 0.000000000000000000 ) ) ;
#16211 = CARTESIAN_POINT ( 'NONE',  ( -42.88789093042842637, 306.3073905683719431, 9.489475012073736337 ) ) ;
#16212 = CARTESIAN_POINT ( 'NONE',  ( -40.53162694259543741, 372.6198905683720000, -11.84573899990672707 ) ) ;
#16213 = CARTESIAN_POINT ( 'NONE',  ( -28.68588794268872988, 517.8698905683720568, 16.75240474999999307 ) ) ;
#16214 = CARTESIAN_POINT ( 'NONE',  ( -10.20829729246298712, 371.6198905601784759, 7.653668647301790529 ) ) ;
#16215 = AXIS2_PLACEMENT_3D ( 'NONE', #8357, #14981, #168 ) ;
#16216 = CARTESIAN_POINT ( 'NONE',  ( -17.35679799567829917, 403.8073905601785327, -16.95518130045146421 ) ) ;
#16217 = ORIENTED_EDGE ( 'NONE', *, *, #10816, .T. ) ;
#16218 = CARTESIAN_POINT ( 'NONE',  ( -14.48388495494901385, 481.3073905683720000, -9.489475012073736337 ) ) ;
#16219 = PRESENTATION_STYLE_ASSIGNMENT (( #2918 ) ) ;
#16220 = CARTESIAN_POINT ( 'NONE',  ( -19.19641293061497578, 280.4323905683720568, -14.20200298773971603 ) ) ;
#16221 = ORIENTED_EDGE ( 'NONE', *, *, #7005, .T. ) ;
#16222 =( BOUNDED_CURVE ( )  B_SPLINE_CURVE ( 2, ( #3165, #2076, #18710, #20453, #2393, #12338, #565, #7133, #10697, #10275, #10592, #20138, #12121, #16895, #8974, #784, #5305 ),
 .UNSPECIFIED., .F., .T. ) 
 B_SPLINE_CURVE_WITH_KNOTS ( ( 3, 2, 2, 2, 2, 2, 2, 2, 3 ),
 ( 0.5625000000000001110, 0.5644531250000001110, 0.5664062500000001110, 0.5683593750000001110, 0.5703125000000001110, 0.5722656250000001110, 0.5742187500000001110, 0.5761718750000001110, 0.5781250000000001110 ),
 .UNSPECIFIED. ) 
 CURVE ( )  GEOMETRIC_REPRESENTATION_ITEM ( )  RATIONAL_B_SPLINE_CURVE ( ( 0.9999999999999988898, 0.9807852804032315408, 1.000000000000000000, 0.9807852804032304306, 1.000000000000000000, 0.9807852804032304306, 1.000000000000000000, 0.9807852804032304306, 1.000000000000000000, 0.9807852804032304306, 1.000000000000000000, 0.9807852804032304306, 1.000000000000000000, 0.9807852804032304306, 1.000000000000000000, 0.9807852804032293204, 1.000000000000001110 ) ) 
 REPRESENTATION_ITEM ( '' )  );
#16223 = CARTESIAN_POINT ( 'NONE',  ( -11.93348319268871194, 290.0573905683720000, 3.332260488124728859 ) ) ;
#16224 = CARTESIAN_POINT ( 'NONE',  ( -42.88789093042842637, 314.8073905683721136, 9.489475012073736337 ) ) ;
#16225 = CARTESIAN_POINT ( 'NONE',  ( -40.53162694259542320, 266.6198905683720568, 11.84573899990672885 ) ) ;
#16226 = CARTESIAN_POINT ( 'NONE',  ( -8.685887942688710339, 257.3073905765656377, -3.978247347593165895 ) ) ;
#16227 = DIRECTION ( 'NONE',  ( -1.191790137725560488E-16, 1.000000000000000000, 0.000000000000000000 ) ) ;
#16228 = CARTESIAN_POINT ( 'NONE',  ( -42.88789093042841927, 232.9323905683720000, -9.489475012073734561 ) ) ;
#16229 = CARTESIAN_POINT ( 'NONE',  ( -22.27502019258948707, 372.2448905683720000, -15.47720386886985544 ) ) ;
#16230 = AXIS2_PLACEMENT_3D ( 'NONE', #12114, #18284, #8439 ) ;
#16231 = CARTESIAN_POINT ( 'NONE',  ( -42.91921849944091605, 203.5275734399367025, 4.734433616062221795 ) ) ;
#16232 = FACE_OUTER_BOUND ( 'NONE', #8346, .T. ) ;
#16233 = ADVANCED_FACE ( 'NONE', ( #9984 ), #18210, .F. ) ;
#16234 = LINE ( 'NONE', #4749, #9080 ) ;
#16235 = EDGE_CURVE ( 'NONE', #1858, #10342, #174, .T. ) ;
#16236 = CARTESIAN_POINT ( 'NONE',  ( -44.16309181155857289, 414.4948905683720000, 6.410867750099241924 ) ) ;
#16237 = CARTESIAN_POINT ( 'NONE',  ( -48.68588794268873698, 573.2448905601785327, 0.000000000000000000 ) ) ;
#16238 = ORIENTED_EDGE ( 'NONE', *, *, #21255, .T. ) ;
#16239 = CARTESIAN_POINT ( 'NONE',  ( -47.16347859291445133, 417.8698905601784759, 7.653668647301805628 ) ) ;
#16240 = ORIENTED_EDGE ( 'NONE', *, *, #19316, .T. ) ;
#16241 = ORIENTED_EDGE ( 'NONE', *, *, #4063, .T. ) ;
#16242 = ORIENTED_EDGE ( 'NONE', *, *, #17683, .F. ) ;
#16243 = CARTESIAN_POINT ( 'NONE',  ( -43.67497163690817530, 210.1113231631600513, -0.6580207156766567644 ) ) ;
#16244 = CARTESIAN_POINT ( 'NONE',  ( -21.03221929538690205, 310.3698905601784759, 18.47759065022572500 ) ) ;
#16245 = DIRECTION ( 'NONE',  ( 0.000000000000000000, 0.000000000000000000, -1.000000000000000000 ) ) ;
#16246 = CARTESIAN_POINT ( 'NONE',  ( -16.84014894278198327, 339.1198905683720568, 11.84573899990672530 ) ) ;
#16247 = CARTESIAN_POINT ( 'NONE',  ( -42.82802356641968089, 510.7448905765656946, -14.14213562373094746 ) ) ;
#16248 = CARTESIAN_POINT ( 'NONE',  ( -45.43829269268871229, 383.8698905683720000, 0.000000000000000000 ) ) ;
#16249 = DIRECTION ( 'NONE',  ( 0.000000000000000000, 0.000000000000000000, -1.000000000000000000 ) ) ;
#16250 = CARTESIAN_POINT ( 'NONE',  ( -28.68588794268871922, 391.3698905683720000, -16.75240474999999307 ) ) ;
#16251 = CARTESIAN_POINT ( 'NONE',  ( -24.70764059509554755, 314.8073905765655809, 19.99999999999998934 ) ) ;
#16252 = CARTESIAN_POINT ( 'NONE',  ( -14.54375231895777709, 423.4948905601784759, -14.14213562373094746 ) ) ;
#16253 = CARTESIAN_POINT ( 'NONE',  ( -25.35362745456397349, 286.6823905683720000, 16.75240474999998952 ) ) ;
#16254 =( NAMED_UNIT ( * ) SI_UNIT ( $, .STERADIAN. ) SOLID_ANGLE_UNIT ( ) );
#16255 = VECTOR ( 'NONE', #12165, 1000.000000000000000 ) ;
#16256 = CIRCLE ( 'NONE', #10111, 22.72497359561857877 ) ;
#16257 = CARTESIAN_POINT ( 'NONE',  ( -40.53162694259544452, 436.6198905683720000, 11.84573899990672885 ) ) ;
#16258 = FACE_OUTER_BOUND ( 'NONE', #1062, .T. ) ;
#16259 = CARTESIAN_POINT ( 'NONE',  ( 0.06682554136337909290, 6.264794173742276762, 2.149058192116895860 ) ) ;
#16260 = CARTESIAN_POINT ( 'NONE',  ( -1.456896669277397076E-16, 0.6351314446025495553, -6.500000000000000000 ) ) ;
#16261 =( GEOMETRIC_REPRESENTATION_CONTEXT ( 3 ) GLOBAL_UNCERTAINTY_ASSIGNED_CONTEXT ( ( #19595 ) ) GLOBAL_UNIT_ASSIGNED_CONTEXT ( ( #4027, #5434, #590 ) ) REPRESENTATION_CONTEXT ( 'NONE', 'WORKASPACE' ) );
#16262 = CARTESIAN_POINT ( 'NONE',  ( -45.43829269268870519, 355.6823905683720000, 3.332260488124734632 ) ) ;
#16263 = CARTESIAN_POINT ( 'NONE',  ( -13.20868407381887799, 499.4948905683720568, -6.410867750099233042 ) ) ;
#16264 = CARTESIAN_POINT ( 'NONE',  ( -36.33955658999052929, 479.1198905601785327, 18.47759065022572500 ) ) ;
#16265 = CARTESIAN_POINT ( 'NONE',  ( -28.68588794268871212, 321.3698905683720568, -16.75240474999999307 ) ) ;
#16266 = EDGE_LOOP ( 'NONE', ( #12453, #9935, #3207, #15633, #14011 ) ) ;
#16267 = AXIS2_PLACEMENT_3D ( 'NONE', #4151, #20497, #1036 ) ;
#16268 = VECTOR ( 'NONE', #15950, 1000.000000000000000 ) ;
#16269 = CARTESIAN_POINT ( 'NONE',  ( -28.68588794268873698, 524.7448905601785327, -19.99999999999999289 ) ) ;
#16270 = ORIENTED_EDGE ( 'NONE', *, *, #15392, .T. ) ;
#16271 = CARTESIAN_POINT ( 'NONE',  ( 0.000000000000000000, 56.85652257517428865, 0.000000000000000000 ) ) ;
#16272 = AXIS2_PLACEMENT_3D ( 'NONE', #13881, #15719, #7468 ) ;
#16273 = CARTESIAN_POINT ( 'NONE',  ( -35.09675569278795138, 403.4948905683720000, -15.47720386886985544 ) ) ;
#16274 = CARTESIAN_POINT ( 'NONE',  ( -22.30770786884145451, 10.52886280891152104, -122.9933582338429972 ) ) ;
#16275 = CARTESIAN_POINT ( 'NONE',  ( -45.43829269268871229, 443.5573905683720000, -3.332260488124726194 ) ) ;
#16276 = VECTOR ( 'NONE', #2787, 1000.000000000000000 ) ;
#16277 = CARTESIAN_POINT ( 'NONE',  ( -16.84014894278199748, 447.6198905683720568, 11.84573899990672530 ) ) ;
#16278 = CARTESIAN_POINT ( 'NONE',  ( 0.000000000000000000, 0.000000000000000000, 0.000000000000000000 ) ) ;
#16279 = DIRECTION ( 'NONE',  ( 0.000000000000000000, 1.000000000000000000, 0.000000000000000000 ) ) ;
#16280 = CARTESIAN_POINT ( 'NONE',  ( -25.35362745456400546, 482.5573905683720000, -16.75240474999999307 ) ) ;
#16281 = CARTESIAN_POINT ( 'NONE',  ( -42.82802356641966668, 390.7448905765656377, -14.14213562373094746 ) ) ;
#16282 = CARTESIAN_POINT ( 'NONE',  ( -28.46624702801777573, 47.09320012170705638, 49.60091809715360256 ) ) ;
#16283 = DIRECTION ( 'NONE',  ( 0.1337298367054296222, -0.9910178256594273094, 0.000000000000000000 ) ) ;
#16284 = CARTESIAN_POINT ( 'NONE',  ( -21.03221929538693047, 428.8698905765655809, -18.47759065022572855 ) ) ;
#16285 = FACE_OUTER_BOUND ( 'NONE', #10877, .T. ) ;
#16286 = CARTESIAN_POINT ( 'NONE',  ( -45.43829269268871940, 495.0573905683719431, -3.332260488124726194 ) ) ;
#16287 = CIRCLE ( 'NONE', #64, 10.00000000000000888 ) ;
#16288 = CARTESIAN_POINT ( 'NONE',  ( 20.42502041961806825, 281.1055109169419666, -40.00000000000000000 ) ) ;
#16289 = VECTOR ( 'NONE', #18319, 1000.000000000000000 ) ;
#16290 = CARTESIAN_POINT ( 'NONE',  ( -40.01497788969912506, 255.6823905601785043, -16.95518130045146421 ) ) ;
#16291 = EDGE_CURVE ( 'NONE', #20443, #17320, #6105, .T. ) ;
#16292 = CARTESIAN_POINT ( 'NONE',  ( -18.68588794268873698, 323.8848358243226357, -20.00000000000000355 ) ) ;
#16293 = CARTESIAN_POINT ( 'NONE',  ( -42.88789093042844058, 406.3073905683719431, 9.489475012073736337 ) ) ;
#16294 = CARTESIAN_POINT ( 'NONE',  ( -21.03221929538692692, 384.1198905601784759, -18.47759065022572855 ) ) ;
#16295 = CARTESIAN_POINT ( 'NONE',  ( -11.93348319268870483, 230.3698905683720284, -2.051577885510841163E-15 ) ) ;
#16296 = ORIENTED_EDGE ( 'NONE', *, *, #923, .F. ) ;
#16297 = PLANE ( 'NONE',  #15509 ) ;
#16298 = ORIENTED_EDGE ( 'NONE', *, *, #1499, .T. ) ;
#16299 = CARTESIAN_POINT ( 'NONE',  ( -32.01814843081345430, 457.5573905683719431, 16.75240474999999307 ) ) ;
#16300 = CARTESIAN_POINT ( 'NONE',  ( -45.64106924314017277, 232.9323905765656093, 11.32908994701042715 ) ) ;
#16301 = ORIENTED_EDGE ( 'NONE', *, *, #20255, .T. ) ;
#16302 = VECTOR ( 'NONE', #5822, 1000.000000000000000 ) ;
#16303 = CARTESIAN_POINT ( 'NONE',  ( -36.33955658999053639, 523.8698905765655809, 18.47759065022572500 ) ) ;
#16304 = CARTESIAN_POINT ( 'NONE',  ( -44.16309181155855867, 223.2448905683720568, -6.410867750099231266 ) ) ;
#16305 = ORIENTED_EDGE ( 'NONE', *, *, #8300, .F. ) ;
#16306 = CARTESIAN_POINT ( 'NONE',  ( -38.17536295476247687, 512.3073905683720568, -14.20200298773971426 ) ) ;
#16307 = FACE_OUTER_BOUND ( 'NONE', #5249, .T. ) ;
#16308 = EDGE_CURVE ( 'NONE', #1090, #1196, #15514, .T. ) ;
#16309 = CARTESIAN_POINT ( 'NONE',  ( -14.54375231895777709, 445.7448905765656377, 14.14213562373094568 ) ) ;
#16310 = LINE ( 'NONE', #13163, #17912 ) ;
#16311 = CARTESIAN_POINT ( 'NONE',  ( -11.93348319268872260, 349.1823905683720000, -3.332260488124732856 ) ) ;
#16312 = CARTESIAN_POINT ( 'NONE',  ( -48.68588794268872277, 451.9948905765656377, 0.000000000000000000 ) ) ;
#16313 = DIRECTION ( 'NONE',  ( 1.000000000000000000, 0.000000000000000000, 0.000000000000000000 ) ) ;
#16314 = CARTESIAN_POINT ( 'NONE',  ( -47.16347859291443712, 287.8698905601784759, 7.653668647301805628 ) ) ;
#16315 = CARTESIAN_POINT ( 'NONE',  ( -22.27502019258946930, 220.7448905683720568, -15.47720386886985544 ) ) ;
#16316 = CARTESIAN_POINT ( 'NONE',  ( -28.68588794268870856, 317.8698905683720000, 16.75240474999999307 ) ) ;
#16317 = DIRECTION ( 'NONE',  ( 0.000000000000000000, 0.000000000000000000, -1.000000000000000000 ) ) ;
#16318 = CARTESIAN_POINT ( 'NONE',  ( -32.66413529028186247, 265.0573905601784759, -19.99999999999999289 ) ) ;
#16319 = CARTESIAN_POINT ( 'NONE',  ( -48.68588794268887199, 377.5573905601785327, 3.978247347592742678 ) ) ;
#16320 = CARTESIAN_POINT ( 'NONE',  ( -25.35362745456398414, 312.5573905683720000, -16.75240474999999307 ) ) ;
#16321 = EDGE_CURVE ( 'NONE', #13474, #11682, #18194, .T. ) ;
#16322 = CARTESIAN_POINT ( 'NONE',  ( -22.27502019258950483, 532.2448905683720568, -15.47720386886985544 ) ) ;
#16323 = CARTESIAN_POINT ( 'NONE',  ( -28.68588794268871567, 364.7448905601784759, -19.99999999999999289 ) ) ;
#16324 = CARTESIAN_POINT ( 'NONE',  ( -17.35679799567828852, 313.8073905601784190, -16.95518130045146421 ) ) ;
#16325 = VERTEX_POINT ( 'NONE', #2009 ) ;
#16326 = CARTESIAN_POINT ( 'NONE',  ( -22.27502019258949062, 478.4948905683720000, 15.47720386886985189 ) ) ;
#16327 = CYLINDRICAL_SURFACE ( 'NONE', #10069, 19.99999999999999645 ) ;
#16328 = CARTESIAN_POINT ( 'NONE',  ( -45.43829269268869808, 283.5573905683720568, -3.332260488124726194 ) ) ;
#16329 = ORIENTED_EDGE ( 'NONE', *, *, #19782, .F. ) ;
#16330 = EDGE_CURVE ( 'NONE', #5058, #19703, #20971, .T. ) ;
#16331 = CARTESIAN_POINT ( 'NONE',  ( -32.01814843081344009, 277.5573905683720568, 16.75240474999999307 ) ) ;
#16332 = CARTESIAN_POINT ( 'NONE',  ( -38.17536295476244845, 312.3073905683720000, -14.20200298773971426 ) ) ;
#16333 = CARTESIAN_POINT ( 'NONE',  ( -19.19641293061496512, 258.8073905683720568, 14.20200298773971426 ) ) ;
#16334 = B_SPLINE_CURVE_WITH_KNOTS ( 'NONE', 3,
 ( #9480, #4616, #5804, #20630, #20852, #7745 ),
 .UNSPECIFIED., .F., .F.,
 ( 4, 2, 4 ),
 ( 0.006874058788776910706, 0.008773169699270546781, 0.01067228060976418286 ),
 .UNSPECIFIED. ) ;
#16335 = CARTESIAN_POINT ( 'NONE',  ( -32.66413529028186247, 254.1823905765655809, 19.99999999999999289 ) ) ;
#16336 = CARTESIAN_POINT ( 'NONE',  ( -17.35679799567830983, 473.8073905601784759, -16.95518130045146421 ) ) ;
#16337 = CARTESIAN_POINT ( 'NONE',  ( -40.53162694259542320, 232.6198905683720000, -11.84573899990672707 ) ) ;
#16338 = CARTESIAN_POINT ( 'NONE',  ( -25.35362745456399480, 382.5573905683720568, -16.75240474999999307 ) ) ;
#16339 = CARTESIAN_POINT ( 'NONE',  ( 91.21585410611801592, 56.85652257517428865, 94.99999999999994316 ) ) ;
#16340 = PRODUCT_DEFINITION_SHAPE ( 'NONE', 'NONE',  #7228 ) ;
#16341 = AXIS2_PLACEMENT_3D ( 'NONE', #5256, #15221, #18345 ) ;
#16342 = CARTESIAN_POINT ( 'NONE',  ( -8.685887942688742314, 573.2448905601785327, 2.449293598294706119E-15 ) ) ;
#16343 = CARTESIAN_POINT ( 'NONE',  ( -22.27502019258949417, 430.7448905683720000, -15.47720386886985544 ) ) ;
#16344 = DIRECTION ( 'NONE',  ( 0.000000000000000000, 0.000000000000000000, 1.000000000000000000 ) ) ;
#16345 = VERTEX_POINT ( 'NONE', #13577 ) ;
#16346 =( BOUNDED_CURVE ( )  B_SPLINE_CURVE ( 2, ( #12377, #14120, #10526, #712, #15852, #8910, #13907, #17253, #7284, #10635, #12275, #9017, #7600, #4266, #9122, #825, #7173 ),
 .UNSPECIFIED., .F., .T. ) 
 B_SPLINE_CURVE_WITH_KNOTS ( ( 3, 2, 2, 2, 2, 2, 2, 2, 3 ),
 ( 0.03125000000000002776, 0.03320312500000007633, 0.03515625000000012490, 0.03710937500000016653, 0.03906250000000021511, 0.04101562500000026368, 0.04296875000000030531, 0.04492187500000035388, 0.04687500000000040246 ),
 .UNSPECIFIED. ) 
 CURVE ( )  GEOMETRIC_REPRESENTATION_ITEM ( )  RATIONAL_B_SPLINE_CURVE ( ( 0.9999999999999997780, 0.9807852804032306526, 1.000000000000000000, 0.9807852804032304306, 1.000000000000000000, 0.9807852804032304306, 1.000000000000000000, 0.9807852804032304306, 1.000000000000000000, 0.9807852804032304306, 1.000000000000000000, 0.9807852804032304306, 1.000000000000000000, 0.9807852804032304306, 1.000000000000000000, 0.9807852804032264338, 1.000000000000003997 ) ) 
 REPRESENTATION_ITEM ( '' )  );
#16347 = CARTESIAN_POINT ( 'NONE',  ( -24.70764059509556887, 424.4323905601784759, -19.99999999999999289 ) ) ;
#16348 = ORIENTED_EDGE ( 'NONE', *, *, #10400, .T. ) ;
#16349 = ORIENTED_EDGE ( 'NONE', *, *, #18779, .F. ) ;
#16350 = VERTEX_POINT ( 'NONE', #494 ) ;
#16351 = CARTESIAN_POINT ( 'NONE',  ( -42.82802356641965957, 353.2448905765656377, 14.14213562373094923 ) ) ;
#16352 = CARTESIAN_POINT ( 'NONE',  ( -32.66413529028186957, 299.4323905601784759, 19.99999999999999289 ) ) ;
#16353 = DIRECTION ( 'NONE',  ( 0.000000000000000000, 1.000000000000000000, 0.000000000000000000 ) ) ;
#16354 = CARTESIAN_POINT ( 'NONE',  ( -32.01814843081344719, 337.5573905683720568, 16.75240474999999307 ) ) ;
#16355 = CARTESIAN_POINT ( 'NONE',  ( -10.20829729246300310, 506.3698905765656946, 7.653668647301790529 ) ) ;
#16356 = CARTESIAN_POINT ( 'NONE',  ( -44.16309181155856578, 384.4948905683720000, 6.410867750099241924 ) ) ;
#16357 = CARTESIAN_POINT ( 'NONE',  ( -35.09675569278795848, 395.7448905683720568, 15.47720386886985366 ) ) ;
#16358 = CARTESIAN_POINT ( 'NONE',  ( -42.82802356641965247, 320.7448905765656377, -14.14213562373094746 ) ) ;
#16359 = CARTESIAN_POINT ( 'NONE',  ( -48.68588794268862330, 426.9323905601784759, -3.978247347593371508 ) ) ;
#16360 = CARTESIAN_POINT ( 'NONE',  ( -13.20868407381884957, 288.2448905683720000, 6.410867750099229490 ) ) ;
#16361 = CARTESIAN_POINT ( 'NONE',  ( 6.416697501590670427, 172.9933428177121471, -60.00000000000000000 ) ) ;
#16362 = CARTESIAN_POINT ( 'NONE',  ( -32.01814843081345430, 433.1823905683721136, -16.75240474999999307 ) ) ;
#16363 = CARTESIAN_POINT ( 'NONE',  ( -28.68588794268875475, 600.7448905601785327, 0.000000000000000000 ) ) ;
#16364 = CARTESIAN_POINT ( 'NONE',  ( 0.000000000000000000, 0.000000000000000000, 40.00000000000000000 ) ) ;
#16365 = PRODUCT_DEFINITION_CONTEXT ( 'detailed design', #13733, 'design' ) ;
#16366 = DIRECTION ( 'NONE',  ( 0.000000000000000000, 1.000000000000000000, -0.000000000000000000 ) ) ;
#16367 = EDGE_CURVE ( 'NONE', #14199, #15635, #6401, .T. ) ;
#16368 = VECTOR ( 'NONE', #13180, 1000.000000000000000 ) ;
#16369 = CARTESIAN_POINT ( 'NONE',  ( -28.68588794268871212, 357.8698905683720568, 16.75240474999999307 ) ) ;
#16370 = CARTESIAN_POINT ( 'NONE',  ( -19.19641293061499354, 487.3073905683719431, 14.20200298773971426 ) ) ;
#16371 = EDGE_CURVE ( 'NONE', #13150, #18908, #12037, .T. ) ;
#16372 = CIRCLE ( 'NONE', #19130, 20.00000000000000000 ) ;
#16373 = ORIENTED_EDGE ( 'NONE', *, *, #18861, .T. ) ;
#16374 = CARTESIAN_POINT ( 'NONE',  ( -24.70764059509556532, 490.0573905601784759, 19.99999999999998934 ) ) ;
#16375 = CARTESIAN_POINT ( 'NONE',  ( -11.93348319268871727, 309.1823905683719431, -3.332260488124732856 ) ) ;
#16376 = EDGE_CURVE ( 'NONE', #10176, #16453, #16144, .T. ) ;
#16377 = ORIENTED_EDGE ( 'NONE', *, *, #13066, .F. ) ;
#16378 = DIRECTION ( 'NONE',  ( 0.000000000000000000, 0.000000000000000000, -1.000000000000000000 ) ) ;
#16379 = VERTEX_POINT ( 'NONE', #5543 ) ;
#16380 = CARTESIAN_POINT ( 'NONE',  ( -30.19626789828514646, 48.38008749069921777, 49.58203932211407761 ) ) ;
#16381 = CARTESIAN_POINT ( 'NONE',  ( -45.43829269268871940, 405.6823905683720568, 3.332260488124734632 ) ) ;
#16382 = CARTESIAN_POINT ( 'NONE',  ( -10.20829729246299600, 446.3698905765656377, 7.653668647301790529 ) ) ;
#16383 = DIRECTION ( 'NONE',  ( -0.000000000000000000, -1.000000000000000000, -0.000000000000000000 ) ) ;
#16384 = CARTESIAN_POINT ( 'NONE',  ( -35.09675569278795138, 441.9948905683720568, -15.47720386886985544 ) ) ;
#16385 = CARTESIAN_POINT ( 'NONE',  ( -40.53162694259544452, 442.6198905683720568, -11.84573899990672707 ) ) ;
#16386 = CARTESIAN_POINT ( 'NONE',  ( -47.16347859291445133, 416.6198905601785327, -7.653668647301793193 ) ) ;
#16387 = ADVANCED_FACE ( 'NONE', ( #698 ), #20057, .F. ) ;
#16388 = CARTESIAN_POINT ( 'NONE',  ( -8.685887942688726326, 386.9948905765655809, -2.449293598294705724E-15 ) ) ;
#16389 = LINE ( 'NONE', #1790, #2391 ) ;
#16390 = CARTESIAN_POINT ( 'NONE',  ( -36.33955658999049376, 265.3698905601784759, -18.47759065022572855 ) ) ;
#16391 = CARTESIAN_POINT ( 'NONE',  ( 65.85920792673738333, 160.1716627696692683, -40.00000000000000000 ) ) ;
#16392 = LINE ( 'NONE', #19304, #3217 ) ;
#16393 = AXIS2_PLACEMENT_3D ( 'NONE', #9692, #13056, #11103 ) ;
#16394 = CARTESIAN_POINT ( 'NONE',  ( -19.19641293061499709, 498.8073905683720000, 14.20200298773971426 ) ) ;
#16395 = LINE ( 'NONE', #21356, #11978 ) ;
#16396 = CARTESIAN_POINT ( 'NONE',  ( -32.66413529028188378, 465.0573905601784190, -19.99999999999999289 ) ) ;
#16397 = CARTESIAN_POINT ( 'NONE',  ( -48.68588794268878672, 517.5573905601784190, 3.978247347593061978 ) ) ;
#16398 = CARTESIAN_POINT ( 'NONE',  ( -25.35362745456398770, 408.1823905683720568, 16.75240474999998952 ) ) ;
#16399 = CARTESIAN_POINT ( 'NONE',  ( -8.685887942688735208, 466.9948905765656377, -2.449293598294705724E-15 ) ) ;
#16400 = CARTESIAN_POINT ( 'NONE',  ( -16.84014894278197261, 239.1198905683720284, 11.84573899990672530 ) ) ;
#16401 = VERTEX_POINT ( 'NONE', #385 ) ;
#16402 = CARTESIAN_POINT ( 'NONE',  ( -11.73070664223725501, 426.0573905765655809, 11.32908994701042005 ) ) ;
#16403 = ORIENTED_EDGE ( 'NONE', *, *, #9299, .F. ) ;
#16404 = CARTESIAN_POINT ( 'NONE',  ( -22.27502019258948707, 438.4948905683720568, 15.47720386886985189 ) ) ;
#16405 = CARTESIAN_POINT ( 'NONE',  ( -48.68588794268869435, 222.3073905765656093, 3.978247347593168115 ) ) ;
#16406 = ORIENTED_EDGE ( 'NONE', *, *, #14403, .F. ) ;
#16407 = DIRECTION ( 'NONE',  ( 0.1639927121256942733, -0.000000000000000000, 0.9864615503757149240 ) ) ;
#16408 = CARTESIAN_POINT ( 'NONE',  ( -22.27502019258945865, 226.9948905683720284, 15.47720386886985189 ) ) ;
#16409 = ORIENTED_EDGE ( 'NONE', *, *, #14921, .F. ) ;
#16410 = CARTESIAN_POINT ( 'NONE',  ( -44.16309181155858710, 503.2448905683719431, -6.410867750099231266 ) ) ;
#16411 = LINE ( 'NONE', #3209, #19028 ) ;
#16412 = CARTESIAN_POINT ( 'NONE',  ( -21.03221929538691981, 445.1198905765655809, 18.47759065022572500 ) ) ;
#16413 = DIRECTION ( 'NONE',  ( 1.191790137725560488E-16, -1.000000000000000000, -0.000000000000000000 ) ) ;
#16414 = CARTESIAN_POINT ( 'NONE',  ( -42.82802356641965247, 328.4948905601784759, 14.14213562373094923 ) ) ;
#16415 = DIRECTION ( 'NONE',  ( 0.000000000000000000, 0.000000000000000000, -1.000000000000000000 ) ) ;
#16416 = CARTESIAN_POINT ( 'NONE',  ( -40.01497788969912506, 240.4323905765656662, -16.95518130045146421 ) ) ;
#16417 = CYLINDRICAL_SURFACE ( 'NONE', #11186, 19.99999999999999645 ) ;
#16418 = CARTESIAN_POINT ( 'NONE',  ( 0.000000000000000000, 31.85652257517428865, 0.000000000000000000 ) ) ;
#16419 = CARTESIAN_POINT ( 'NONE',  ( -43.04611869048239470, 202.6362012587621280, -4.338193544061892837 ) ) ;
#16420 = CARTESIAN_POINT ( 'NONE',  ( -14.48388495494899075, 309.4323905683720568, 9.489475012073732785 ) ) ;
#16421 = CARTESIAN_POINT ( 'NONE',  ( -11.73070664223726034, 443.1823905601784759, -11.32908994701042538 ) ) ;
#16422 = CARTESIAN_POINT ( 'NONE',  ( -36.33955658999049376, 265.3698905601784759, -18.47759065022572855 ) ) ;
#16423 = CYLINDRICAL_SURFACE ( 'NONE', #9200, 49.93977357075243617 ) ;
#16424 = CARTESIAN_POINT ( 'NONE',  ( -35.09675569278793716, 293.4948905683720000, -15.47720386886985544 ) ) ;
#16425 = EDGE_CURVE ( 'NONE', #15077, #16081, #13675, .T. ) ;
#16426 = CARTESIAN_POINT ( 'NONE',  ( -11.93348319268874036, 520.6823905683719431, -3.332260488124732856 ) ) ;
#16427 = CARTESIAN_POINT ( 'NONE',  ( -48.68588794268870856, 357.2448905601784759, 0.000000000000000000 ) ) ;
#16428 = FACE_OUTER_BOUND ( 'NONE', #20872, .T. ) ;
#16429 = VERTEX_POINT ( 'NONE', #17027 ) ;
#16430 = CARTESIAN_POINT ( 'NONE',  ( -16.84014894278200458, 481.6198905683720000, -11.84573899990672707 ) ) ;
#16431 = EDGE_CURVE ( 'NONE', #763, #7305, #7267, .T. ) ;
#16432 = CARTESIAN_POINT ( 'NONE',  ( -1.025382690249029949, 160.1716627696692683, 25.00000000000000000 ) ) ;
#16433 = CARTESIAN_POINT ( 'NONE',  ( -11.93348319268871194, 278.5573905683720000, 3.332260488124728415 ) ) ;
#16434 = VERTEX_POINT ( 'NONE', #5653 ) ;
#16435 = CARTESIAN_POINT ( 'NONE',  ( -38.17536295476244845, 283.8073905683720568, -14.20200298773971426 ) ) ;
#16436 = CARTESIAN_POINT ( 'NONE',  ( -45.43829269268869808, 255.3698905683720000, 0.000000000000000000 ) ) ;
#16437 = CARTESIAN_POINT ( 'NONE',  ( -21.03221929538690915, 238.8698905765656093, -18.47759065022572855 ) ) ;
#16438 = DIRECTION ( 'NONE',  ( 1.232945044042657126E-32, -9.855701800883825964E-17, 1.000000000000000000 ) ) ;
#16439 = EDGE_CURVE ( 'NONE', #18143, #14497, #10512, .T. ) ;
#16440 = CARTESIAN_POINT ( 'NONE',  ( -11.93348319268870661, 229.1823905683720568, -3.332260488124732856 ) ) ;
#16441 = CARTESIAN_POINT ( 'NONE',  ( -14.48388495494898898, 269.8073905683720000, -9.489475012073736337 ) ) ;
#16442 = CARTESIAN_POINT ( 'NONE',  ( -44.16309181155857289, 384.7448905683720000, -6.410867750099231266 ) ) ;
#16443 = CARTESIAN_POINT ( 'NONE',  ( 18.55315245287936321, 326.0737056351150613, -25.00000000000000000 ) ) ;
#16444 = CARTESIAN_POINT ( 'NONE',  ( 45.67500000000000426, 0.000000000000000000, 3.309499999999999886 ) ) ;
#16445 = CARTESIAN_POINT ( 'NONE',  ( -48.68588794268870146, 271.9948905765656377, 0.000000000000000000 ) ) ;
#16446 = EDGE_CURVE ( 'NONE', #9649, #3515, #5463, .T. ) ;
#16447 = CARTESIAN_POINT ( 'NONE',  ( -38.17536295476245556, 415.4323905683720568, 14.20200298773971781 ) ) ;
#16448 = DIRECTION ( 'NONE',  ( -1.000000000000000000, 0.000000000000000000, 0.000000000000000000 ) ) ;
#16449 = ORIENTED_EDGE ( 'NONE', *, *, #18119, .F. ) ;
#16450 = CARTESIAN_POINT ( 'NONE',  ( -10.20829729246299244, 422.8698905601784759, -7.653668647301794969 ) ) ;
#16451 = ORIENTED_EDGE ( 'NONE', *, *, #17469, .T. ) ;
#16452 = CARTESIAN_POINT ( 'NONE',  ( 18.55315245287936321, 130.1716627696692683, 25.00000000000000000 ) ) ;
#16453 = VERTEX_POINT ( 'NONE', #7478 ) ;
#16454 = EDGE_LOOP ( 'NONE', ( #15739, #3671, #5310 ) ) ;
#16455 = CARTESIAN_POINT ( 'NONE',  ( -8.685887942688985675, 356.6823905765654672, 3.978247347593800054 ) ) ;
#16456 = CARTESIAN_POINT ( 'NONE',  ( -17.35679799567829207, 303.8073905601784759, -16.95518130045146421 ) ) ;
#16457 = DIRECTION ( 'NONE',  ( 1.000000000000000000, 0.000000000000000000, -0.000000000000000000 ) ) ;
#16458 = CARTESIAN_POINT ( 'NONE',  ( -44.16309181155857289, 334.7448905683720568, -6.410867750099231266 ) ) ;
#16459 = CARTESIAN_POINT ( 'NONE',  ( -42.82802356641967378, 493.2448905765656377, 14.14213562373094923 ) ) ;
#16460 = CARTESIAN_POINT ( 'NONE',  ( -25.35362745456399125, 371.0573905683720000, -16.75240474999999307 ) ) ;
#16461 = FACE_OUTER_BOUND ( 'NONE', #20729, .T. ) ;
#16462 = CARTESIAN_POINT ( 'NONE',  ( -11.93348319268872260, 378.8698905683720000, -2.051577885510841163E-15 ) ) ;
#16463 = EDGE_CURVE ( 'NONE', #14441, #9372, #12790, .T. ) ;
#16464 = CARTESIAN_POINT ( 'NONE',  ( -47.16347859291443712, 302.6198905765656377, 7.653668647301805628 ) ) ;
#16465 = FACE_OUTER_BOUND ( 'NONE', #13558, .T. ) ;
#16466 = CARTESIAN_POINT ( 'NONE',  ( -19.19641293061497223, 280.4323905683720568, -14.20200298773971603 ) ) ;
#16467 = CYLINDRICAL_SURFACE ( 'NONE', #14298, 19.99999999999999645 ) ;
#16468 = CARTESIAN_POINT ( 'NONE',  ( -35.09675569278795848, 437.2448905683720000, 15.47720386886985366 ) ) ;
#16469 = VECTOR ( 'NONE', #3167, 1000.000000000000227 ) ;
#16470 = LINE ( 'NONE', #17962, #1646 ) ;
#16471 = CARTESIAN_POINT ( 'NONE',  ( 20.42502041961813575, 271.1055109169419666, 40.00000000000000000 ) ) ;
#16472 = CARTESIAN_POINT ( 'NONE',  ( -48.68588794268872277, 481.9948905765656377, 0.000000000000000000 ) ) ;
#16473 =( BOUNDED_CURVE ( )  B_SPLINE_CURVE ( 2, ( #12776, #16455, #12887, #19369, #21309, #8098, #1746, #8210, #2937, #4657, #9624, #11461, #16351, #9941, #9517, #19793, #3147 ),
 .UNSPECIFIED., .F., .T. ) 
 B_SPLINE_CURVE_WITH_KNOTS ( ( 3, 2, 2, 2, 2, 2, 2, 2, 3 ),
 ( 0.5468750000000003331, 0.5488281250000003331, 0.5507812500000002220, 0.5527343750000002220, 0.5546875000000002220, 0.5566406250000002220, 0.5585937500000002220, 0.5605468750000001110, 0.5625000000000001110 ),
 .UNSPECIFIED. ) 
 CURVE ( )  GEOMETRIC_REPRESENTATION_ITEM ( )  RATIONAL_B_SPLINE_CURVE ( ( 0.9999999999999966693, 0.9807852804032337612, 1.000000000000000000, 0.9807852804032304306, 1.000000000000000000, 0.9807852804032304306, 1.000000000000000000, 0.9807852804032304306, 1.000000000000000000, 0.9807852804032304306, 1.000000000000000000, 0.9807852804032304306, 1.000000000000000000, 0.9807852804032304306, 1.000000000000000000, 0.9807852804032293204, 1.000000000000001110 ) ) 
 REPRESENTATION_ITEM ( '' )  );
#16474 = DIRECTION ( 'NONE',  ( 0.000000000000000000, 0.000000000000000000, -1.000000000000000000 ) ) ;
#16475 = EDGE_CURVE ( 'NONE', #15642, #7137, #11396, .T. ) ;
#16476 = CARTESIAN_POINT ( 'NONE',  ( -40.53162694259543741, 356.6198905683720000, 11.84573899990672885 ) ) ;
#16477 = CARTESIAN_POINT ( 'NONE',  ( -16.84014894278200458, 480.1198905683720000, -11.84573899990672707 ) ) ;
#16478 = ORIENTED_EDGE ( 'NONE', *, *, #19536, .F. ) ;
#16479 = CARTESIAN_POINT ( 'NONE',  ( -48.68588794268872277, 486.9323905601785327, -3.978247347593158345 ) ) ;
#16480 = CARTESIAN_POINT ( 'NONE',  ( -45.43829269268869808, 294.1823905683720000, 3.332260488124734632 ) ) ;
#16481 = VECTOR ( 'NONE', #13815, 1000.000000000000000 ) ;
#16482 = VERTEX_POINT ( 'NONE', #10838 ) ;
#16483 = CARTESIAN_POINT ( 'NONE',  ( -10.20829729246298356, 346.3698905765655809, 7.653668647301790529 ) ) ;
#16484 = ORIENTED_EDGE ( 'NONE', *, *, #12363, .F. ) ;
#16485 = DIRECTION ( 'NONE',  ( 0.3512089204514979301, 0.000000000000000000, -0.9362971185447991340 ) ) ;
#16486 = AXIS2_PLACEMENT_3D ( 'NONE', #20509, #10433, #17055 ) ;
#16487 = CARTESIAN_POINT ( 'NONE',  ( -22.27502019258948351, 408.4948905683720000, 15.47720386886985189 ) ) ;
#16488 = CARTESIAN_POINT ( 'NONE',  ( -24.70764059509556176, 480.0573905601784759, 19.99999999999998934 ) ) ;
#16489 = CARTESIAN_POINT ( 'NONE',  ( -40.53162694259544452, 425.1198905683720000, 11.84573899990672885 ) ) ;
#16490 = CARTESIAN_POINT ( 'NONE',  ( -19.19641293061498999, 447.3073905683720568, 14.20200298773971426 ) ) ;
#16491 = CARTESIAN_POINT ( 'NONE',  ( 51.98438129372387806, 30.52886280891151216, -117.7249735956185219 ) ) ;
#16492 = CARTESIAN_POINT ( 'NONE',  ( -14.54375231895776821, 375.7448905765656377, 14.14213562373094568 ) ) ;
#16493 = CARTESIAN_POINT ( 'NONE',  ( -17.27065617357490268, 46.46077788388278407, 48.27172322967895468 ) ) ;
#16494 = CARTESIAN_POINT ( 'NONE',  ( -42.82802356641966668, 390.7448905765656377, -14.14213562373094746 ) ) ;
#16495 = DIRECTION ( 'NONE',  ( 0.000000000000000000, 0.000000000000000000, 1.000000000000000000 ) ) ;
#16496 = CARTESIAN_POINT ( 'NONE',  ( 5.700000000000000178, 4.898587196589412829E-16, -4.000000000000000000 ) ) ;
#16497 = CARTESIAN_POINT ( 'NONE',  ( -35.09675569278795848, 503.4948905683720568, -15.47720386886985544 ) ) ;
#16498 = AXIS2_PLACEMENT_3D ( 'NONE', #1149, #7720, #17573 ) ;
#16499 = CARTESIAN_POINT ( 'NONE',  ( -33.07955326574332133, 600.7448905601785327, 10.74819839862556492 ) ) ;
#16500 = LINE ( 'NONE', #13141, #3109 ) ;
#16501 = CARTESIAN_POINT ( 'NONE',  ( -28.68588794268871922, 419.7448905601784759, 19.99999999999999289 ) ) ;
#16502 = VECTOR ( 'NONE', #9187, 1000.000000000000000 ) ;
#16503 = CARTESIAN_POINT ( 'NONE',  ( -45.43829269268871940, 415.3698905683720568, 0.000000000000000000 ) ) ;
#16504 = CARTESIAN_POINT ( 'NONE',  ( -28.68588794268872988, 469.4948905765656377, -19.99999999999999289 ) ) ;
#16505 = EDGE_CURVE ( 'NONE', #19523, #20734, #21012, .T. ) ;
#16506 = CARTESIAN_POINT ( 'NONE',  ( -25.35362745456397704, 232.5573905683720568, -16.75240474999999307 ) ) ;
#16507 = EDGE_CURVE ( 'NONE', #3879, #11996, #9214, .T. ) ;
#16508 = ORIENTED_EDGE ( 'NONE', *, *, #15019, .T. ) ;
#16509 = DIRECTION ( 'NONE',  ( 3.836511174089486666E-16, 0.000000000000000000, -1.000000000000000000 ) ) ;
#16510 = EDGE_LOOP ( 'NONE', ( #10522, #20848, #17113, #13012 ) ) ;
#16511 = CARTESIAN_POINT ( 'NONE',  ( -45.43829269268871940, 435.0573905683720568, -3.332260488124726638 ) ) ;
#16512 = CARTESIAN_POINT ( 'NONE',  ( -42.88789093042845479, 532.9323905683720568, -9.489475012073736337 ) ) ;
#16513 = EDGE_LOOP ( 'NONE', ( #3171, #12936 ) ) ;
#16514 = CARTESIAN_POINT ( 'NONE',  ( -28.68588794268874054, 608.2448905601786464, 20.00000000000000000 ) ) ;
#16515 = CARTESIAN_POINT ( 'NONE',  ( -42.88789093042841927, 224.8073905683720284, 9.489475012073736337 ) ) ;
#16516 = ORIENTED_EDGE ( 'NONE', *, *, #16208, .T. ) ;
#16517 = CARTESIAN_POINT ( 'NONE',  ( -35.09675569278796559, 511.9948905683720000, -15.47720386886985544 ) ) ;
#16518 = CARTESIAN_POINT ( 'NONE',  ( -43.68588794268873698, 588.2448905601785327, 1.836970198721029589E-15 ) ) ;
#16519 = CARTESIAN_POINT ( 'NONE',  ( -21.03221929538691981, 435.1198905765656377, 18.47759065022572500 ) ) ;
#16520 = CARTESIAN_POINT ( 'NONE',  ( -14.54375231895776999, 358.2448905765656377, -14.14213562373094746 ) ) ;
#16521 = CARTESIAN_POINT ( 'NONE',  ( -36.33955658999049376, 250.1198905765656377, -18.47759065022572855 ) ) ;
#16522 = CARTESIAN_POINT ( 'NONE',  ( 5.074999999999999289, 6.500000000000000888, 0.000000000000000000 ) ) ;
#16523 = CARTESIAN_POINT ( 'NONE',  ( 158.8141120573112630, 610.7448905601785327, 0.000000000000000000 ) ) ;
#16524 = FACE_BOUND ( 'NONE', #2885, .T. ) ;
#16525 = CARTESIAN_POINT ( 'NONE',  ( 0.2565376335220210802, -2.516992571281988056, -6.499999999999999112 ) ) ;
#16526 = CARTESIAN_POINT ( 'NONE',  ( -48.68588794268872277, 477.2448905601784759, 0.000000000000000000 ) ) ;
#16527 = CARTESIAN_POINT ( 'NONE',  ( -44.16309181155856578, 304.7448905683720568, -6.410867750099231266 ) ) ;
#16528 = LINE ( 'NONE', #94, #16812 ) ;
#16529 = CARTESIAN_POINT ( 'NONE',  ( -21.03221929538689849, 260.3698905601785327, 18.47759065022572500 ) ) ;
#16530 = CARTESIAN_POINT ( 'NONE',  ( -14.54375231895777354, 415.7448905765655809, 14.14213562373094568 ) ) ;
#16531 = CARTESIAN_POINT ( 'NONE',  ( -38.17536295476246977, 503.8073905683721136, -14.20200298773971426 ) ) ;
#16532 =( BOUNDED_CURVE ( )  B_SPLINE_CURVE ( 2, ( #14983, #9870, #17786, #17991, #8359, #19725, #11184, #170, #1352, #14877, #16284, #13025, #6312, #16175, #4692, #1459, #3401 ),
 .UNSPECIFIED., .F., .T. ) 
 B_SPLINE_CURVE_WITH_KNOTS ( ( 3, 2, 2, 2, 2, 2, 2, 2, 3 ),
 ( 0.3125000000000001110, 0.3144531250000001110, 0.3164062500000001110, 0.3183593750000001110, 0.3203125000000001110, 0.3222656250000001110, 0.3242187500000001110, 0.3261718750000001110, 0.3281250000000001110 ),
 .UNSPECIFIED. ) 
 CURVE ( )  GEOMETRIC_REPRESENTATION_ITEM ( )  RATIONAL_B_SPLINE_CURVE ( ( 0.9999999999999988898, 0.9807852804032315408, 1.000000000000000000, 0.9807852804032304306, 1.000000000000000000, 0.9807852804032304306, 1.000000000000000000, 0.9807852804032304306, 1.000000000000000000, 0.9807852804032304306, 1.000000000000000000, 0.9807852804032304306, 1.000000000000000000, 0.9807852804032304306, 1.000000000000000000, 0.9807852804032293204, 1.000000000000001110 ) ) 
 REPRESENTATION_ITEM ( '' )  );
#16533 = CARTESIAN_POINT ( 'NONE',  ( -48.68588794268870856, 366.9323905601785327, -3.978247347593158345 ) ) ;
#16534 = CARTESIAN_POINT ( 'NONE',  ( -48.68588794268873698, 573.2448905601785327, 0.000000000000000000 ) ) ;
#16535 = ORIENTED_EDGE ( 'NONE', *, *, #11869, .T. ) ;
#16536 = CARTESIAN_POINT ( 'NONE',  ( -19.19641293061499709, 471.9323905683720568, -14.20200298773971603 ) ) ;
#16537 = DIRECTION ( 'NONE',  ( 1.000000000000000000, 0.000000000000000000, 0.000000000000000000 ) ) ;
#16538 = CARTESIAN_POINT ( 'NONE',  ( -19.19641293061497578, 287.3073905683720000, 14.20200298773971426 ) ) ;
#16539 = ORIENTED_EDGE ( 'NONE', *, *, #5565, .F. ) ;
#16540 = DIRECTION ( 'NONE',  ( -1.191790137725560488E-16, 1.000000000000000000, -0.000000000000000000 ) ) ;
#16541 = CARTESIAN_POINT ( 'NONE',  ( -45.43829269268870519, 285.6823905683720000, 3.332260488124734632 ) ) ;
#16542 = CARTESIAN_POINT ( 'NONE',  ( -14.48388495494898720, 261.3073905683720568, -9.489475012073734561 ) ) ;
#16543 = CARTESIAN_POINT ( 'NONE',  ( -47.16347859291443001, 242.6198905765656377, 7.653668647301805628 ) ) ;
#16544 = CARTESIAN_POINT ( 'NONE',  ( -17.35679799567830273, 418.5573905765655809, -16.95518130045146421 ) ) ;
#16545 = CARTESIAN_POINT ( 'NONE',  ( -48.68588794268869435, 237.2448905601785043, 0.000000000000000000 ) ) ;
#16546 = DIRECTION ( 'NONE',  ( 3.836511174089486173E-16, -0.000000000000000000, 1.000000000000000000 ) ) ;
#16547 = CARTESIAN_POINT ( 'NONE',  ( -38.17536295476243424, 265.4323905683720568, 14.20200298773971781 ) ) ;
#16548 = CARTESIAN_POINT ( 'NONE',  ( -11.93348319268872260, 370.3698905683720568, -2.051577885510841163E-15 ) ) ;
#16549 = CARTESIAN_POINT ( 'NONE',  ( -28.68588794268874054, 573.2448905601785327, 0.000000000000000000 ) ) ;
#16550 = DIRECTION ( 'NONE',  ( 0.000000000000000000, -1.000000000000000000, 0.000000000000000000 ) ) ;
#16551 = EDGE_CURVE ( 'NONE', #2936, #13, #1126, .T. ) ;
#16552 = CARTESIAN_POINT ( 'NONE',  ( -17.35679799567828496, 268.5573905765656377, -16.95518130045146421 ) ) ;
#16553 = CARTESIAN_POINT ( 'NONE',  ( -38.17536295476246266, 432.3073905683720000, -14.20200298773971426 ) ) ;
#16554 = UNCERTAINTY_MEASURE_WITH_UNIT (LENGTH_MEASURE( 1.000000000000000082E-05 ), #1343, 'distance_accuracy_value', 'NONE');
#16555 = CARTESIAN_POINT ( 'NONE',  ( 4.700000000000000178, 3.752776749732560368, -6.499999999999999112 ) ) ;
#16556 = EDGE_LOOP ( 'NONE', ( #17804, #7357, #11597, #3673 ) ) ;
#16557 = CARTESIAN_POINT ( 'NONE',  ( -8.685887942688729879, 432.2448905601785327, -2.449293598294705724E-15 ) ) ;
#16558 = VERTEX_POINT ( 'NONE', #1022 ) ;
#16559 = CARTESIAN_POINT ( 'NONE',  ( -28.68588794268875120, 585.7448905601785327, 0.000000000000000000 ) ) ;
#16560 = VERTEX_POINT ( 'NONE', #10940 ) ;
#16561 = ORIENTED_EDGE ( 'NONE', *, *, #10537, .T. ) ;
#16562 = CARTESIAN_POINT ( 'NONE',  ( 4.700000000000000178, 3.752776749732563033, 6.500000000000000000 ) ) ;
#16563 = CARTESIAN_POINT ( 'NONE',  ( -28.68588794268870501, 309.7448905601785327, 19.99999999999999289 ) ) ;
#16564 = CARTESIAN_POINT ( 'NONE',  ( 151.4788465195079823, 620.7448905601785327, -8.917803138848077182 ) ) ;
#16565 = CARTESIAN_POINT ( 'NONE',  ( -13.20868407381885667, 349.7448905683720568, 6.410867750099229490 ) ) ;
#16566 = ORIENTED_EDGE ( 'NONE', *, *, #17344, .F. ) ;
#16567 = CARTESIAN_POINT ( 'NONE',  ( -8.685887942688736985, 486.9948905765656377, -2.449293598294705724E-15 ) ) ;
#16568 = CARTESIAN_POINT ( 'NONE',  ( -16.84014894278199037, 370.1198905683720000, -11.84573899990672707 ) ) ;
#16569 = CARTESIAN_POINT ( 'NONE',  ( -38.17536295476245556, 395.4323905683720000, 14.20200298773971781 ) ) ;
#16570 = AXIS2_PLACEMENT_3D ( 'NONE', #18705, #15165, #3891 ) ;
#16571 = EDGE_CURVE ( 'NONE', #14089, #11949, #7488, .T. ) ;
#16572 = CARTESIAN_POINT ( 'NONE',  ( -8.685887942688715668, 307.3073905765655809, -3.978247347593165895 ) ) ;
#16573 = FACE_OUTER_BOUND ( 'NONE', #15478, .T. ) ;
#16574 = CARTESIAN_POINT ( 'NONE',  ( -11.93348319268871194, 289.1823905683720000, -3.332260488124732856 ) ) ;
#16575 = CARTESIAN_POINT ( 'NONE',  ( -8.685887942688729879, 442.2448905601785327, -2.449293598294705724E-15 ) ) ;
#16576 = CARTESIAN_POINT ( 'NONE',  ( -22.27502019258948351, 428.4948905683720568, 15.47720386886985189 ) ) ;
#16577 = CARTESIAN_POINT ( 'NONE',  ( -28.68588794268872277, 250.8848358243226357, -20.00000000000000000 ) ) ;
#16578 = CARTESIAN_POINT ( 'NONE',  ( -10.20829729246300310, 501.6198905601785327, 7.653668647301790529 ) ) ;
#16579 = PLANE ( 'NONE',  #1606 ) ;
#16580 = DIRECTION ( 'NONE',  ( 0.000000000000000000, 1.000000000000000000, -0.000000000000000000 ) ) ;
#16581 = CARTESIAN_POINT ( 'NONE',  ( -14.48388495494899786, 351.3073905683721136, -9.489475012073736337 ) ) ;
#16582 = CARTESIAN_POINT ( 'NONE',  ( -45.43829269268872650, 473.8698905683720568, 0.000000000000000000 ) ) ;
#16583 = ORIENTED_EDGE ( 'NONE', *, *, #18034, .T. ) ;
#16584 = CARTESIAN_POINT ( 'NONE',  ( -8.685887942688736985, 482.5573905601784759, -3.978247347593165895 ) ) ;
#16585 = CARTESIAN_POINT ( 'NONE',  ( -32.01814843081344009, 311.6823905683720568, -16.75240474999999307 ) ) ;
#16586 = AXIS2_PLACEMENT_3D ( 'NONE', #13302, #5174, #10349 ) ;
#16587 = EDGE_CURVE ( 'NONE', #8775, #4755, #20802, .T. ) ;
#16588 = DIRECTION ( 'NONE',  ( -9.855701800883827197E-17, 1.000000000000000000, 0.000000000000000000 ) ) ;
#16589 = ORIENTED_EDGE ( 'NONE', *, *, #3542, .F. ) ;
#16590 = FACE_OUTER_BOUND ( 'NONE', #9328, .T. ) ;
#16591 = CARTESIAN_POINT ( 'NONE',  ( -28.68588794268871567, 397.8698905683720000, 16.75240474999999307 ) ) ;
#16592 = CARTESIAN_POINT ( 'NONE',  ( -42.82802356641966668, 443.2448905765656377, 14.14213562373094923 ) ) ;
#16593 = CARTESIAN_POINT ( 'NONE',  ( -28.68588794268871567, 384.4948905765656377, 19.99999999999999289 ) ) ;
#16594 = CARTESIAN_POINT ( 'NONE',  ( -38.17536295476245556, 415.4323905683720568, 14.20200298773971781 ) ) ;
#16595 = CARTESIAN_POINT ( 'NONE',  ( -19.19641293061497223, 268.8073905683720568, 14.20200298773971426 ) ) ;
#16596 = CARTESIAN_POINT ( 'NONE',  ( -11.93348319268872970, 438.5573905683720000, 3.332260488124728859 ) ) ;
#16597 = PRODUCT_CONTEXT ( 'NONE', #14970, 'mechanical' ) ;
#16598 = DIRECTION ( 'NONE',  ( -1.191790137725560488E-16, 1.000000000000000000, -0.000000000000000000 ) ) ;
#16599 = ADVANCED_FACE ( 'NONE', ( #12583 ), #17550, .T. ) ;
#16600 = CARTESIAN_POINT ( 'NONE',  ( -45.64106924314018698, 361.0573905765656946, -11.32908994701042715 ) ) ;
#16601 = CARTESIAN_POINT ( 'NONE',  ( -28.68588794268872633, 250.8848358243226357, 0.000000000000000000 ) ) ;
#16602 = PLANE ( 'NONE',  #13953 ) ;
#16603 = CARTESIAN_POINT ( 'NONE',  ( -14.31911992702480241, 600.7448905601785327, 19.70857778461545351 ) ) ;
#16604 =( BOUNDED_CURVE ( )  B_SPLINE_CURVE ( 2, ( #5666, #10525, #930, #17147, #10421, #18855, #15743, #14119, #2224, #15851, #10852, #5879, #10742, #13906, #5451, #2435, #12376 ),
 .UNSPECIFIED., .F., .T. ) 
 B_SPLINE_CURVE_WITH_KNOTS ( ( 3, 2, 2, 2, 2, 2, 2, 2, 3 ),
 ( 0.7500000000000001110, 0.7519531250000001110, 0.7539062500000001110, 0.7558593750000001110, 0.7578125000000001110, 0.7597656250000001110, 0.7617187500000001110, 0.7636718750000001110, 0.7656250000000001110 ),
 .UNSPECIFIED. ) 
 CURVE ( )  GEOMETRIC_REPRESENTATION_ITEM ( )  RATIONAL_B_SPLINE_CURVE ( ( 0.9999999999999988898, 0.9807852804032315408, 1.000000000000000000, 0.9807852804032304306, 1.000000000000000000, 0.9807852804032304306, 1.000000000000000000, 0.9807852804032304306, 1.000000000000000000, 0.9807852804032304306, 1.000000000000000000, 0.9807852804032304306, 1.000000000000000000, 0.9807852804032304306, 1.000000000000000000, 0.9807852804032293204, 1.000000000000001110 ) ) 
 REPRESENTATION_ITEM ( '' )  );
#16605 = CARTESIAN_POINT ( 'NONE',  ( -16.84014894278200813, 501.6198905683720000, -11.84573899990672707 ) ) ;
#16606 = B_SPLINE_CURVE_WITH_KNOTS ( 'NONE', 3,
 ( #5594, #18172, #7314, #18574, #3370, #12197 ),
 .UNSPECIFIED., .F., .F.,
 ( 4, 2, 4 ),
 ( 2.380733003139562229E-07, 0.001898835937927375282, 0.003797433802554436334 ),
 .UNSPECIFIED. ) ;
#16607 = CARTESIAN_POINT ( 'NONE',  ( -28.68588794268874054, 271.1055109169419666, 40.00000000000000000 ) ) ;
#16608 = CARTESIAN_POINT ( 'NONE',  ( -40.01497788969915348, 518.8073905601785327, 16.95518130045146776 ) ) ;
#16609 = AXIS2_PLACEMENT_3D ( 'NONE', #14785, #16407, #17697 ) ;
#16610 = CARTESIAN_POINT ( 'NONE',  ( -13.20868407381886556, 410.9948905683720000, -6.410867750099233042 ) ) ;
#16611 = CARTESIAN_POINT ( 'NONE',  ( -23.06691706883066928, 45.31613216062292082, -122.8556579767893027 ) ) ;
#16612 = CARTESIAN_POINT ( 'NONE',  ( -22.27502019258946220, 238.4948905683720284, 15.47720386886985189 ) ) ;
#16613 = CARTESIAN_POINT ( 'NONE',  ( -25.35362745456398059, 356.6823905683720568, 16.75240474999998952 ) ) ;
#16614 = EDGE_LOOP ( 'NONE', ( #5446, #6831, #20067, #13962 ) ) ;
#16615 = CARTESIAN_POINT ( 'NONE',  ( -11.93348319268874036, 518.5573905683720568, 3.332260488124728415 ) ) ;
#16616 = EDGE_LOOP ( 'NONE', ( #5690, #4426, #8771, #7741, #19898 ) ) ;
#16617 = CARTESIAN_POINT ( 'NONE',  ( -11.93348319268872970, 440.3698905683720000, -2.051577885510841163E-15 ) ) ;
#16618 = AXIS2_PLACEMENT_3D ( 'NONE', #19001, #8938, #12195 ) ;
#16619 = CARTESIAN_POINT ( 'NONE',  ( -14.48388495494901917, 529.8073905683720568, -9.489475012073736337 ) ) ;
#16620 = ORIENTED_EDGE ( 'NONE', *, *, #1382, .F. ) ;
#16621 = CARTESIAN_POINT ( 'NONE',  ( -8.685887942688820473, 431.9323905601784190, 3.978247347593374172 ) ) ;
#16622 = CARTESIAN_POINT ( 'NONE',  ( -40.53162694259545162, 492.6198905683720000, -11.84573899990672707 ) ) ;
#16623 = VERTEX_POINT ( 'NONE', #17656 ) ;
#16624 = CARTESIAN_POINT ( 'NONE',  ( -45.43829269268872650, 503.5573905683720000, -3.332260488124726638 ) ) ;
#16625 = CARTESIAN_POINT ( 'NONE',  ( -23.82844689576343100, 45.41375816275737520, -49.36319628876446330 ) ) ;
#16626 = VECTOR ( 'NONE', #20921, 999.9999999999998863 ) ;
#16628 = VECTOR ( 'NONE', #5097, 1000.000000000000000 ) ;
#16627 = CARTESIAN_POINT ( 'NONE',  ( -45.64106924314019409, 431.0573905765655809, -11.32908994701042715 ) ) ;
#16629 = CARTESIAN_POINT ( 'NONE',  ( -28.68588794268872633, 250.8848358243226357, 20.00000000000000000 ) ) ;
#16630 = FACE_OUTER_BOUND ( 'NONE', #10976, .T. ) ;
#16631 = CARTESIAN_POINT ( 'NONE',  ( -45.64106924314019409, 452.9323905765656377, 11.32908994701042538 ) ) ;
#16632 = CYLINDRICAL_SURFACE ( 'NONE', #11476, 4.000000000000001776 ) ;
#16633 = ADVANCED_FACE ( 'NONE', ( #16049 ), #17761, .T. ) ;
#16634 = DIRECTION ( 'NONE',  ( -1.000000000000000000, -1.191790137725560488E-16, 0.000000000000000000 ) ) ;
#16635 = CARTESIAN_POINT ( 'NONE',  ( 60.03793209889851568, 30.52886280891152282, -136.1729372809869005 ) ) ;
#16636 = CARTESIAN_POINT ( 'NONE',  ( -43.37414277151795261, 201.1719893629813498, -3.054701555947804792 ) ) ;
#16637 = AXIS2_PLACEMENT_3D ( 'NONE', #4187, #14263, #4403 ) ;
#16638 = CARTESIAN_POINT ( 'NONE',  ( -14.48388495494899075, 291.3073905683720568, -9.489475012073736337 ) ) ;
#16639 = DIRECTION ( 'NONE',  ( -0.000000000000000000, -0.000000000000000000, -1.000000000000000000 ) ) ;
#16640 = CARTESIAN_POINT ( 'NONE',  ( -28.68588794268870501, 264.7448905601784759, -19.99999999999999289 ) ) ;
#16641 = CARTESIAN_POINT ( 'NONE',  ( -29.07862423524327156, 47.49931253676632537, -49.60091809715360256 ) ) ;
#16642 = CARTESIAN_POINT ( 'NONE',  ( -45.43829269268870519, 285.3698905683720568, 0.000000000000000000 ) ) ;
#16643 = EDGE_CURVE ( 'NONE', #5454, #16087, #18953, .T. ) ;
#16644 = VECTOR ( 'NONE', #16675, 1000.000000000000227 ) ;
#16645 = CARTESIAN_POINT ( 'NONE',  ( -45.64106924314020119, 536.3073905601785327, -11.32908994701042538 ) ) ;
#16646 = CARTESIAN_POINT ( 'NONE',  ( -35.09675569278796559, 497.2448905683720000, 15.47720386886985366 ) ) ;
#16647 = EDGE_CURVE ( 'NONE', #5288, #13870, #4991, .T. ) ;
#16648 = EDGE_CURVE ( 'NONE', #18441, #8749, #1067, .T. ) ;
#16649 = DIRECTION ( 'NONE',  ( -1.191790137725560488E-16, 1.000000000000000000, -0.000000000000000000 ) ) ;
#16650 = ORIENTED_EDGE ( 'NONE', *, *, #9568, .F. ) ;
#16651 = CARTESIAN_POINT ( 'NONE',  ( -16.84014894278200103, 469.1198905683720568, 11.84573899990672530 ) ) ;
#16652 = CARTESIAN_POINT ( 'NONE',  ( -24.70764059509556532, 409.1823905765656377, -19.99999999999999289 ) ) ;
#16653 = CARTESIAN_POINT ( 'NONE',  ( -16.84014894278197616, 267.6198905683720568, 11.84573899990672530 ) ) ;
#16654 = ORIENTED_EDGE ( 'NONE', *, *, #12536, .F. ) ;
#16655 = CARTESIAN_POINT ( 'NONE',  ( 125.7989814974898053, 10.52886280891152104, -40.00000000000000000 ) ) ;
#16656 = CARTESIAN_POINT ( 'NONE',  ( -14.48388495494898542, 241.3073905683720568, -9.489475012073734561 ) ) ;
#16657 = EDGE_CURVE ( 'NONE', #5663, #14938, #13225, .T. ) ;
#16658 = CARTESIAN_POINT ( 'NONE',  ( -40.01497788969911795, 253.5573905765656093, 16.95518130045146776 ) ) ;
#16659 = FACE_OUTER_BOUND ( 'NONE', #16078, .T. ) ;
#16660 = CARTESIAN_POINT ( 'NONE',  ( -47.16347859291443001, 227.8698905601784759, 7.653668647301805628 ) ) ;
#16661 = CARTESIAN_POINT ( 'NONE',  ( -47.16347859291443001, 261.3698905765656377, -7.653668647301793193 ) ) ;
#16662 = CARTESIAN_POINT ( 'NONE',  ( -25.35362745456398059, 261.0573905683720000, -16.75240474999999307 ) ) ;
#16663 = CARTESIAN_POINT ( 'NONE',  ( -11.93348319268872260, 350.0573905683720000, 3.332260488124728415 ) ) ;
#16664 = CARTESIAN_POINT ( 'NONE',  ( -47.16347859291443712, 277.8698905601784759, 7.653668647301805628 ) ) ;
#16665 =( BOUNDED_CURVE ( )  B_SPLINE_CURVE ( 2, ( #13760, #16794, #2079, #5307, #361, #3587, #6822, #8553, #11803, #20140, #11908, #20346, #20455, #5206, #12123, #10173, #13438 ),
 .UNSPECIFIED., .F., .T. ) 
 B_SPLINE_CURVE_WITH_KNOTS ( ( 3, 2, 2, 2, 2, 2, 2, 2, 3 ),
 ( 0.3906250000000001665, 0.3925781250000001665, 0.3945312500000001665, 0.3964843750000001665, 0.3984375000000001665, 0.4003906250000001665, 0.4023437500000001665, 0.4042968750000001665, 0.4062500000000001665 ),
 .UNSPECIFIED. ) 
 CURVE ( )  GEOMETRIC_REPRESENTATION_ITEM ( )  RATIONAL_B_SPLINE_CURVE ( ( 0.9999999999999983347, 0.9807852804032320959, 1.000000000000000000, 0.9807852804032304306, 1.000000000000000000, 0.9807852804032304306, 1.000000000000000000, 0.9807852804032304306, 1.000000000000000000, 0.9807852804032304306, 1.000000000000000000, 0.9807852804032304306, 1.000000000000000000, 0.9807852804032304306, 1.000000000000000000, 0.9807852804032287652, 1.000000000000001554 ) ) 
 REPRESENTATION_ITEM ( '' )  );
#16666 = CARTESIAN_POINT ( 'NONE',  ( -32.01814843081345430, 421.6823905683720568, -16.75240474999999307 ) ) ;
#16667 = DIRECTION ( 'NONE',  ( 0.000000000000000000, 0.000000000000000000, 1.000000000000000000 ) ) ;
#16668 = ORIENTED_EDGE ( 'NONE', *, *, #2214, .T. ) ;
#16669 = CARTESIAN_POINT ( 'NONE',  ( -21.03221929538693047, 414.1198905601785327, -18.47759065022572855 ) ) ;
#16670 = ORIENTED_EDGE ( 'NONE', *, *, #4468, .T. ) ;
#16671 = DIRECTION ( 'NONE',  ( 0.000000000000000000, 0.000000000000000000, -1.000000000000000000 ) ) ;
#16672 = ORIENTED_EDGE ( 'NONE', *, *, #18440, .F. ) ;
#16673 = CARTESIAN_POINT ( 'NONE',  ( -19.19641293061500420, 521.9323905683720568, -14.20200298773971603 ) ) ;
#16674 = CARTESIAN_POINT ( 'NONE',  ( -47.16347859291443712, 307.8698905601784759, 7.653668647301805628 ) ) ;
#16675 = DIRECTION ( 'NONE',  ( -0.3512089204514986518, 0.000000000000000000, 0.9362971185447986899 ) ) ;
#16676 = AXIS2_PLACEMENT_3D ( 'NONE', #20570, #19264, #9197 ) ;
#16677 = CARTESIAN_POINT ( 'NONE',  ( -25.35362745456398770, 322.5573905683720000, -16.75240474999999307 ) ) ;
#16678 = CARTESIAN_POINT ( 'NONE',  ( -28.68588794268871212, 356.3698905683720568, 16.75240474999999307 ) ) ;
#16679 = CARTESIAN_POINT ( 'NONE',  ( -28.68588794268871567, 361.3698905683720568, -16.75240474999999307 ) ) ;
#16680 = CARTESIAN_POINT ( 'NONE',  ( -11.73070664223724258, 297.9323905765655240, -11.32908994701042715 ) ) ;
#16681 = LINE ( 'NONE', #11693, #3101 ) ;
#16682 = CARTESIAN_POINT ( 'NONE',  ( -45.43829269268870519, 274.1823905683720000, 3.332260488124734632 ) ) ;
#16683 = CARTESIAN_POINT ( 'NONE',  ( -28.68588794268872277, 439.7448905601784759, 19.99999999999999289 ) ) ;
#16684 = AXIS2_PLACEMENT_3D ( 'NONE', #21141, #19514, #3078 ) ;
#16685 = CARTESIAN_POINT ( 'NONE',  ( -38.17536295476245556, 426.9323905683720000, 14.20200298773971781 ) ) ;
#16686 = CYLINDRICAL_SURFACE ( 'NONE', #18903, 19.99999999999999645 ) ;
#16687 = CARTESIAN_POINT ( 'NONE',  ( -28.68588794268874409, 608.2448905601786464, 0.000000000000000000 ) ) ;
#16688 = DIRECTION ( 'NONE',  ( -1.191790137725560488E-16, 1.000000000000000000, -0.000000000000000000 ) ) ;
#16689 = CARTESIAN_POINT ( 'NONE',  ( 60.03793209889851568, 10.52886280891152104, -126.1729372809868863 ) ) ;
#16690 = CARTESIAN_POINT ( 'NONE',  ( -38.17536295476244845, 323.8073905683719431, -14.20200298773971426 ) ) ;
#16691 = CARTESIAN_POINT ( 'NONE',  ( -40.53162694259545162, 485.1198905683720000, 11.84573899990672885 ) ) ;
#16692 = ORIENTED_EDGE ( 'NONE', *, *, #19748, .T. ) ;
#16693 = CARTESIAN_POINT ( 'NONE',  ( -8.685887942688738761, 492.5573905601785327, -3.978247347593165895 ) ) ;
#16694 = CARTESIAN_POINT ( 'NONE',  ( -16.84014894278198327, 310.1198905683720000, -11.84573899990672707 ) ) ;
#16695 = EDGE_CURVE ( 'NONE', #2403, #18883, #16470, .T. ) ;
#16696 = CARTESIAN_POINT ( 'NONE',  ( -8.685887942688720997, 342.2448905601784759, -2.449293598294705724E-15 ) ) ;
#16697 = ORIENTED_EDGE ( 'NONE', *, *, #3927, .T. ) ;
#16698 = CARTESIAN_POINT ( 'NONE',  ( -48.68588794268873698, 573.2448905601785327, 0.000000000000000000 ) ) ;
#16699 = MECHANICAL_DESIGN_GEOMETRIC_PRESENTATION_REPRESENTATION (  '', ( #13601 ), #10121 ) ;
#16700 = CARTESIAN_POINT ( 'NONE',  ( -22.27502019258949062, 402.2448905683720568, -15.47720386886985544 ) ) ;
#16701 = CARTESIAN_POINT ( 'NONE',  ( -36.33955658999052929, 479.1198905601785327, 18.47759065022572500 ) ) ;
#16702 = CARTESIAN_POINT ( 'NONE',  ( -40.01497788969913216, 383.5573905765656377, 16.95518130045146776 ) ) ;
#16703 = CARTESIAN_POINT ( 'NONE',  ( -22.27502019258949417, 430.7448905683720000, -15.47720386886985544 ) ) ;
#16704 = CARTESIAN_POINT ( 'NONE',  ( -42.88789093042841927, 256.3073905683720568, 9.489475012073736337 ) ) ;
#16705 = ADVANCED_BREP_SHAPE_REPRESENTATION ( '', ( #4901, #12794 ), #13835 ) ;
#16706 = CARTESIAN_POINT ( 'NONE',  ( -42.88789093042844058, 424.8073905683719431, 9.489475012073734561 ) ) ;
#16707 = LINE ( 'NONE', #19834, #8035 ) ;
#16708 = CARTESIAN_POINT ( 'NONE',  ( -14.54375231895777176, 368.2448905765656377, -14.14213562373094746 ) ) ;
#16709 = CARTESIAN_POINT ( 'NONE',  ( -42.82802356641965247, 275.9948905601785327, -14.14213562373094746 ) ) ;
#16710 = DIRECTION ( 'NONE',  ( 0.000000000000000000, 0.000000000000000000, -1.000000000000000000 ) ) ;
#16711 = CARTESIAN_POINT ( 'NONE',  ( -38.17536295476244845, 335.4323905683720000, 14.20200298773971781 ) ) ;
#16712 = DIRECTION ( 'NONE',  ( 0.000000000000000000, -1.000000000000000000, 0.000000000000000000 ) ) ;
#16713 = CARTESIAN_POINT ( 'NONE',  ( -11.93348319268873681, 490.0573905683720568, 3.332260488124728415 ) ) ;
#16714 = EDGE_CURVE ( 'NONE', #7492, #10771, #3164, .T. ) ;
#16715 = AXIS2_PLACEMENT_3D ( 'NONE', #7656, #19238, #2806 ) ;
#16716 = PLANE ( 'NONE',  #4387 ) ;
#16717 = CARTESIAN_POINT ( 'NONE',  ( -43.66427838156418062, 210.0786766341574889, 0.8210443013742925178 ) ) ;
#16718 = VECTOR ( 'NONE', #9766, 1000.000000000000000 ) ;
#16719 = CARTESIAN_POINT ( 'NONE',  ( -25.35362745456398414, 398.1823905683720568, 16.75240474999998952 ) ) ;
#16720 = CARTESIAN_POINT ( 'NONE',  ( -48.68588794268869435, 261.9948905765655809, 0.000000000000000000 ) ) ;
#16721 = CARTESIAN_POINT ( 'NONE',  ( -44.16309181155855867, 224.7448905683720568, -6.410867750099231266 ) ) ;
#16722 = CARTESIAN_POINT ( 'NONE',  ( -19.19641293061498644, 360.4323905683720000, -14.20200298773971603 ) ) ;
#16723 = ADVANCED_FACE ( 'NONE', ( #19696 ), #19813, .T. ) ;
#16724 = ORIENTED_EDGE ( 'NONE', *, *, #4648, .T. ) ;
#16725 = CARTESIAN_POINT ( 'NONE',  ( -13.20868407381887977, 519.4948905683720568, -6.410867750099233042 ) ) ;
#16726 = ORIENTED_EDGE ( 'NONE', *, *, #13647, .T. ) ;
#16727 = CARTESIAN_POINT ( 'NONE',  ( -35.09675569278795138, 443.4948905683720568, -15.47720386886985544 ) ) ;
#16728 = CARTESIAN_POINT ( 'NONE',  ( -38.17536295476246977, 515.4323905683720568, 14.20200298773971781 ) ) ;
#16729 = AXIS2_PLACEMENT_3D ( 'NONE', #8907, #10740, #9229 ) ;
#16730 = VERTEX_POINT ( 'NONE', #16577 ) ;
#16731 = CARTESIAN_POINT ( 'NONE',  ( 60.03793209889851568, 10.52886280891152104, 131.1729372809869005 ) ) ;
#16732 = CARTESIAN_POINT ( 'NONE',  ( -25.35362745456400901, 491.0573905683720000, -16.75240474999999307 ) ) ;
#16733 = ORIENTED_EDGE ( 'NONE', *, *, #10344, .F. ) ;
#16734 = CARTESIAN_POINT ( 'NONE',  ( -22.27502019258949417, 506.9948905683721136, 15.47720386886985189 ) ) ;
#16735 = CARTESIAN_POINT ( 'NONE',  ( -24.85718862968342435, 45.58919278729139535, -49.45561310859971371 ) ) ;
#16736 = CIRCLE ( 'NONE', #17418, 4.000000000000000000 ) ;
#16737 = CARTESIAN_POINT ( 'NONE',  ( -17.35679799567830628, 428.5573905765656377, -16.95518130045146421 ) ) ;
#16738 = CARTESIAN_POINT ( 'NONE',  ( -32.66413529028186957, 359.8073905765656946, -19.99999999999999289 ) ) ;
#16739 = CYLINDRICAL_SURFACE ( 'NONE', #13042, 4.000000000000001776 ) ;
#16740 = CARTESIAN_POINT ( 'NONE',  ( 78.68120802659204571, 149.7457237375499517, -20.00000000000000355 ) ) ;
#16741 = DIRECTION ( 'NONE',  ( -1.191790137725560488E-16, 1.000000000000000000, -0.000000000000000000 ) ) ;
#16742 = CARTESIAN_POINT ( 'NONE',  ( 0.01372220897662189062, -5.948365447239590154, -2.697128823393882158 ) ) ;
#16743 = DIRECTION ( 'NONE',  ( 1.000000000000000000, 0.000000000000000000, -0.000000000000000000 ) ) ;
#16744 = CARTESIAN_POINT ( 'NONE',  ( -42.93756312153262655, 203.3739285472156268, -4.679109617540635924 ) ) ;
#16745 = CARTESIAN_POINT ( 'NONE',  ( -25.35362745456397349, 288.1823905683720000, 16.75240474999998952 ) ) ;
#16746 = CARTESIAN_POINT ( 'NONE',  ( -42.82802356641968089, 528.4948905601785327, 14.14213562373094923 ) ) ;
#16747 = CARTESIAN_POINT ( 'NONE',  ( -47.16347859291443001, 266.6198905601784759, -7.653668647301793193 ) ) ;
#16748 = LINE ( 'NONE', #20092, #20622 ) ;
#16749 = VECTOR ( 'NONE', #6832, 1000.000000000000000 ) ;
#16750 = CARTESIAN_POINT ( 'NONE',  ( -40.53162694259543031, 284.1198905683720000, -11.84573899990672707 ) ) ;
#16751 = ORIENTED_EDGE ( 'NONE', *, *, #18350, .T. ) ;
#16752 = CARTESIAN_POINT ( 'NONE',  ( -22.30770786884145451, 30.52886280891152282, 122.9933582338429972 ) ) ;
#16753 = CARTESIAN_POINT ( 'NONE',  ( -14.48388495494901385, 509.4323905683720000, 9.489475012073731008 ) ) ;
#16754 = VERTEX_POINT ( 'NONE', #8006 ) ;
#16755 = CARTESIAN_POINT ( 'NONE',  ( -11.93348319268873325, 460.3698905683720000, -2.051577885510841163E-15 ) ) ;
#16756 = CARTESIAN_POINT ( 'NONE',  ( -11.73070664223725501, 407.9323905765656377, -11.32908994701042538 ) ) ;
#16757 = CARTESIAN_POINT ( 'NONE',  ( -32.01814843081343298, 261.6823905683720568, -16.75240474999999307 ) ) ;
#16758 = ORIENTED_EDGE ( 'NONE', *, *, #14701, .F. ) ;
#16759 = CARTESIAN_POINT ( 'NONE',  ( -21.03221929538690560, 335.1198905765655809, 18.47759065022572500 ) ) ;
#16760 = CARTESIAN_POINT ( 'NONE',  ( -25.35362745456397704, 252.5573905683720000, -16.75240474999999307 ) ) ;
#16761 = CARTESIAN_POINT ( 'NONE',  ( -21.03221929538689849, 245.1198905765656377, 18.47759065022572500 ) ) ;
#16762 = DIRECTION ( 'NONE',  ( -0.000000000000000000, -1.000000000000000000, -0.000000000000000000 ) ) ;
#16763 = CARTESIAN_POINT ( 'NONE',  ( -42.82802356641964536, 235.9948905601784759, -14.14213562373094746 ) ) ;
#16764 = CARTESIAN_POINT ( 'NONE',  ( -22.27502019258946575, 276.9948905683720000, 15.47720386886985189 ) ) ;
#16765 = EDGE_CURVE ( 'NONE', #20871, #20201, #9743, .T. ) ;
#16766 = CARTESIAN_POINT ( 'NONE',  ( -38.17536295476245556, 353.8073905683720568, -14.20200298773971426 ) ) ;
#16767 = CARTESIAN_POINT ( 'NONE',  ( -28.68588794268873343, 504.7448905601785896, -19.99999999999999289 ) ) ;
#16768 = APPLICATION_CONTEXT ( 'automotive_design' ) ;
#16769 = CARTESIAN_POINT ( 'NONE',  ( -16.84014894278199037, 397.6198905683720568, 11.84573899990672530 ) ) ;
#16770 = CYLINDRICAL_SURFACE ( 'NONE', #204, 10.00000000000000888 ) ;
#16771 = EDGE_LOOP ( 'NONE', ( #15668, #11780 ) ) ;
#16772 = CARTESIAN_POINT ( 'NONE',  ( -42.82802356641966668, 398.4948905601784759, 14.14213562373094923 ) ) ;
#16773 = ADVANCED_FACE ( 'NONE', ( #16258 ), #18181, .F. ) ;
#16774 = VERTEX_POINT ( 'NONE', #8333 ) ;
#16775 = B_SPLINE_CURVE_WITH_KNOTS ( 'NONE', 3,
 ( #2771, #12611, #4281, #19203, #4385, #3082, #1154, #21039, #1252, #10970, #6003, #15863, #7616, #17686, #17578, #14561, #11292, #4596, #21146, #9353, #15968, #14458, #12716, #944 ),
 .UNSPECIFIED., .F., .F.,
 ( 4, 2, 2, 2, 2, 2, 2, 2, 2, 2, 2, 4 ),
 ( 0.000000000000000000, 0.002720743832753576025, 0.005441487665507152051, 0.006801859581883942449, 0.008162231498260731979, 0.01088297533101431798, 0.01224334724739110924, 0.01360371916376789878, 0.01632446299652147784, 0.01768483491289826390, 0.01904520682927505343, 0.02176595066202864637 ),
 .UNSPECIFIED. ) ;
#16776 = ORIENTED_EDGE ( 'NONE', *, *, #3329, .T. ) ;
#16777 = EDGE_LOOP ( 'NONE', ( #6270, #15157 ) ) ;
#16778 = CARTESIAN_POINT ( 'NONE',  ( -28.68588794268873698, 522.8698905683719431, -16.75240474999999307 ) ) ;
#16779 = CARTESIAN_POINT ( 'NONE',  ( -8.685887942688713892, 292.5573905601784759, -3.978247347593165895 ) ) ;
#16780 = CARTESIAN_POINT ( 'NONE',  ( -43.31958977256851995, 208.9114094701607485, -3.303159798271271708 ) ) ;
#16781 = CARTESIAN_POINT ( 'NONE',  ( -38.17536295476244845, 323.8073905683720000, -14.20200298773971426 ) ) ;
#16782 = ORIENTED_EDGE ( 'NONE', *, *, #21383, .F. ) ;
#16783 = CARTESIAN_POINT ( 'NONE',  ( -38.17536295476244845, 355.4323905683720568, 14.20200298773971781 ) ) ;
#16784 = CARTESIAN_POINT ( 'NONE',  ( -16.84014894278199037, 370.1198905683720000, -11.84573899990672707 ) ) ;
#16785 = CARTESIAN_POINT ( 'NONE',  ( -40.01497788969912506, 303.5573905765656377, 16.95518130045146776 ) ) ;
#16786 = CYLINDRICAL_SURFACE ( 'NONE', #16230, 22.72497359561857877 ) ;
#16787 = CARTESIAN_POINT ( 'NONE',  ( -11.93348319268870839, 258.5573905683720000, 3.332260488124728859 ) ) ;
#16788 = DIRECTION ( 'NONE',  ( 0.000000000000000000, -0.000000000000000000, 1.000000000000000000 ) ) ;
#16789 =( BOUNDED_CURVE ( )  B_SPLINE_CURVE ( 2, ( #7484, #3319, #13164, #6438, #6869, #3426, #8272, #1704, #196, #1819, #19751, #6546, #16414, #1592, #18234, #4934, #15118 ),
 .UNSPECIFIED., .F., .T. ) 
 B_SPLINE_CURVE_WITH_KNOTS ( ( 3, 2, 2, 2, 2, 2, 2, 2, 3 ),
 ( 0.6406250000000002220, 0.6425781250000002220, 0.6445312500000002220, 0.6464843750000001110, 0.6484375000000001110, 0.6503906250000001110, 0.6523437500000000000, 0.6542968750000000000, 0.6562500000000000000 ),
 .UNSPECIFIED. ) 
 CURVE ( )  GEOMETRIC_REPRESENTATION_ITEM ( )  RATIONAL_B_SPLINE_CURVE ( ( 0.9999999999999977796, 0.9807852804032326510, 1.000000000000000000, 0.9807852804032304306, 1.000000000000000000, 0.9807852804032304306, 1.000000000000000000, 0.9807852804032304306, 1.000000000000000000, 0.9807852804032304306, 1.000000000000000000, 0.9807852804032304306, 1.000000000000000000, 0.9807852804032304306, 1.000000000000000000, 0.9807852804032304306, 1.000000000000000000 ) ) 
 REPRESENTATION_ITEM ( '' )  );
#16790 = CARTESIAN_POINT ( 'NONE',  ( -19.19641293061498999, 421.9323905683720000, -14.20200298773971603 ) ) ;
#16791 = CARTESIAN_POINT ( 'NONE',  ( -48.68588794268873698, 573.2448905601785327, 0.000000000000000000 ) ) ;
#16792 = DIRECTION ( 'NONE',  ( 0.000000000000000000, 0.000000000000000000, 1.000000000000000000 ) ) ;
#16793 = CARTESIAN_POINT ( 'NONE',  ( -8.685887942688722774, 362.2448905601784190, -2.449293598294705724E-15 ) ) ;
#16794 = CARTESIAN_POINT ( 'NONE',  ( -8.685887942688859553, 411.9323905601784190, 3.978247347593479866 ) ) ;
#16795 = CARTESIAN_POINT ( 'NONE',  ( -13.20868407381885312, 319.7448905683720000, 6.410867750099229490 ) ) ;
#16796 = CARTESIAN_POINT ( 'NONE',  ( -38.17536295476246266, 475.4323905683720568, 14.20200298773971781 ) ) ;
#16797 = ORIENTED_EDGE ( 'NONE', *, *, #5110, .F. ) ;
#16798 = CARTESIAN_POINT ( 'NONE',  ( -47.16347859291445843, 457.8698905601785327, 7.653668647301805628 ) ) ;
#16799 = CARTESIAN_POINT ( 'NONE',  ( -45.43829269268869808, 313.5573905683720000, -3.332260488124726194 ) ) ;
#16800 = CARTESIAN_POINT ( 'NONE',  ( 0.5805565836007606784, -3.752776749732561701, 6.500000000000000000 ) ) ;
#16801 = ORIENTED_EDGE ( 'NONE', *, *, #1134, .T. ) ;
#16802 = DIRECTION ( 'NONE',  ( -1.250996701150283068E-16, 1.000000000000000000, 0.000000000000000000 ) ) ;
#16803 = CARTESIAN_POINT ( 'NONE',  ( -36.33955658999050797, 345.3698905601784759, -18.47759065022572855 ) ) ;
#16804 = CARTESIAN_POINT ( 'NONE',  ( -28.68588794268871922, 392.8698905683720000, -16.75240474999999307 ) ) ;
#16805 = CARTESIAN_POINT ( 'NONE',  ( -123.2946569474810019, 30.52886280891154058, -20.57735571454641388 ) ) ;
#16806 = CYLINDRICAL_SURFACE ( 'NONE', #16978, 19.99999999999999645 ) ;
#16807 = CARTESIAN_POINT ( 'NONE',  ( -45.43829269268871229, 424.1823905683721136, 3.332260488124734632 ) ) ;
#16808 = CARTESIAN_POINT ( 'NONE',  ( -32.01814843081343298, 263.1823905683720000, -16.75240474999999307 ) ) ;
#16809 = CARTESIAN_POINT ( 'NONE',  ( -16.84014894278199748, 430.1198905683720000, -11.84573899990672707 ) ) ;
#16810 = PRODUCT_CONTEXT ( 'NONE', #6103, 'mechanical' ) ;
#16811 = CARTESIAN_POINT ( 'NONE',  ( 60.03793209889851568, 30.52886280891152282, 131.1729372809869005 ) ) ;
#16812 = VECTOR ( 'NONE', #20090, 1000.000000000000000 ) ;
#16813 = CARTESIAN_POINT ( 'NONE',  ( -11.73070664223724968, 366.0573905765655809, 11.32908994701042005 ) ) ;
#16814 = CARTESIAN_POINT ( 'NONE',  ( -8.685887942688720997, 346.9948905765656377, -2.449293598294705724E-15 ) ) ;
#16815 = CARTESIAN_POINT ( 'NONE',  ( -6.276925316985672687, 600.7448905601785327, -44.69718552705352721 ) ) ;
#16816 = CARTESIAN_POINT ( 'NONE',  ( -42.88789093042842637, 324.8073905683720000, 9.489475012073734561 ) ) ;
#16817 = LINE ( 'NONE', #20054, #6571 ) ;
#16818 = CARTESIAN_POINT ( 'NONE',  ( -21.03221929538691981, 435.1198905765656377, 18.47759065022572500 ) ) ;
#16819 =( LENGTH_UNIT ( ) NAMED_UNIT ( * ) SI_UNIT ( .MILLI., .METRE. ) );
#16820 = CARTESIAN_POINT ( 'NONE',  ( -45.64106924314017277, 306.3073905601784190, -11.32908994701042538 ) ) ;
#16821 = CIRCLE ( 'NONE', #11958, 210.7252770684331438 ) ;
#16822 = CARTESIAN_POINT ( 'NONE',  ( -38.17536295476245556, 383.8073905683720568, -14.20200298773971426 ) ) ;
#16823 = CARTESIAN_POINT ( 'NONE',  ( -28.68588794268873698, -129.7637193493918915, 0.000000000000000000 ) ) ;
#16824 = EDGE_CURVE ( 'NONE', #3730, #9937, #2011, .T. ) ;
#16825 = CARTESIAN_POINT ( 'NONE',  ( -32.66413529028189799, 529.4323905601785327, 19.99999999999999289 ) ) ;
#16826 = CARTESIAN_POINT ( 'NONE',  ( -16.84014894278198682, 357.6198905683720000, 11.84573899990672530 ) ) ;
#16827 = CONICAL_SURFACE ( 'NONE', #13000, 6.500000000000000000, 1.047197551196600296 ) ;
#16828 = VERTEX_POINT ( 'NONE', #1437 ) ;
#16829 = CARTESIAN_POINT ( 'NONE',  ( -22.27502019258949773, 526.9948905683720568, 15.47720386886985189 ) ) ;
#16830 = ORIENTED_EDGE ( 'NONE', *, *, #10549, .F. ) ;
#16831 = CARTESIAN_POINT ( 'NONE',  ( -16.84014894278201169, 520.1198905683720568, -11.84573899990672707 ) ) ;
#16832 = ORIENTED_EDGE ( 'NONE', *, *, #5370, .F. ) ;
#16833 = CARTESIAN_POINT ( 'NONE',  ( -21.03221929538694113, 494.1198905601784759, -18.47759065022572855 ) ) ;
#16834 = CARTESIAN_POINT ( 'NONE',  ( -40.53162694259545162, 485.1198905683720000, 11.84573899990672885 ) ) ;
#16835 = ORIENTED_EDGE ( 'NONE', *, *, #13079, .T. ) ;
#16836 = CARTESIAN_POINT ( 'NONE',  ( -22.27502019258949062, 486.9948905683720568, 15.47720386886985189 ) ) ;
#16837 = CARTESIAN_POINT ( 'NONE',  ( -28.25075301531890304, 46.95029017519802750, -49.60091809715360966 ) ) ;
#16838 = VECTOR ( 'NONE', #20726, 1000.000000000000000 ) ;
#16839 = CARTESIAN_POINT ( 'NONE',  ( -32.66413529028188378, 429.8073905765656946, -19.99999999999999289 ) ) ;
#16840 = LINE ( 'NONE', #15330, #14827 ) ;
#16841 = CARTESIAN_POINT ( 'NONE',  ( 20.74841189052422052, 585.7448905601785327, -7.500000000000000000 ) ) ;
#16842 = CARTESIAN_POINT ( 'NONE',  ( -32.66413529028187668, 439.8073905765656946, -19.99999999999999289 ) ) ;
#16843 = FACE_OUTER_BOUND ( 'NONE', #10048, .T. ) ;
#16844 = ADVANCED_FACE ( 'NONE', ( #14640 ), #13001, .T. ) ;
#16845 = AXIS2_PLACEMENT_3D ( 'NONE', #3191, #17996, #6315 ) ;
#16846 = CARTESIAN_POINT ( 'NONE',  ( -42.82802356641966668, 435.9948905601784759, -14.14213562373094746 ) ) ;
#16847 = CARTESIAN_POINT ( 'NONE',  ( -10.20829729246300310, 496.3698905765655809, 7.653668647301790529 ) ) ;
#16848 = CARTESIAN_POINT ( 'NONE',  ( -25.35362745456397349, 298.1823905683720000, 16.75240474999998952 ) ) ;
#16849 = DIRECTION ( 'NONE',  ( 0.000000000000000000, 0.000000000000000000, -1.000000000000000000 ) ) ;
#16850 = CARTESIAN_POINT ( 'NONE',  ( -14.48388495494900852, 441.3073905683720568, -9.489475012073736337 ) ) ;
#16851 = CARTESIAN_POINT ( 'NONE',  ( -22.27502019258946930, 288.4948905683720000, 15.47720386886985189 ) ) ;
#16852 = VECTOR ( 'NONE', #11446, 999.9999999999998863 ) ;
#16853 = ORIENTED_EDGE ( 'NONE', *, *, #20462, .F. ) ;
#16854 = CARTESIAN_POINT ( 'NONE',  ( -28.68588794268875120, 610.7448905601785327, 0.000000000000000000 ) ) ;
#16855 = CARTESIAN_POINT ( 'NONE',  ( -14.48388495494901562, 501.3073905683720568, -9.489475012073734561 ) ) ;
#16856 = EDGE_CURVE ( 'NONE', #15800, #11839, #15255, .T. ) ;
#16857 = VECTOR ( 'NONE', #17734, 1000.000000000000000 ) ;
#16858 = ORIENTED_EDGE ( 'NONE', *, *, #3832, .F. ) ;
#16859 = CARTESIAN_POINT ( 'NONE',  ( -11.93348319268873503, 470.6823905683720568, -3.332260488124732856 ) ) ;
#16860 = CARTESIAN_POINT ( 'NONE',  ( 43.53705524234220547, 56.85652257517428865, -96.62835994548002816 ) ) ;
#16861 = CARTESIAN_POINT ( 'NONE',  ( -45.43829269268869098, 254.1823905683719715, 3.332260488124734632 ) ) ;
#16862 = VERTEX_POINT ( 'NONE', #20344 ) ;
#16863 = CARTESIAN_POINT ( 'NONE',  ( 6.416697501590670427, 217.7548513357008630, 49.99999999999999289 ) ) ;
#16864 = DIRECTION ( 'NONE',  ( -1.000000000000000000, 0.000000000000000000, 0.000000000000000000 ) ) ;
#16865 = CARTESIAN_POINT ( 'NONE',  ( -44.16309181155855157, 245.9948905683720284, 6.410867750099241924 ) ) ;
#16866 = ADVANCED_FACE ( 'NONE', ( #10379 ), #18498, .T. ) ;
#16867 = CARTESIAN_POINT ( 'NONE',  ( -10.20829729246297823, 311.6198905601784759, 7.653668647301790529 ) ) ;
#16868 = DIRECTION ( 'NONE',  ( 1.000000000000000000, 0.000000000000000000, 0.000000000000000000 ) ) ;
#16869 = CARTESIAN_POINT ( 'NONE',  ( -13.20868407381884779, 268.2448905683720568, 6.410867750099229490 ) ) ;
#16870 = CARTESIAN_POINT ( 'NONE',  ( -14.48388495494899786, 359.4323905683719431, 9.489475012073732785 ) ) ;
#16871 = CARTESIAN_POINT ( 'NONE',  ( -17.35679799567831338, 503.8073905601785327, -16.95518130045146421 ) ) ;
#16872 = CARTESIAN_POINT ( 'NONE',  ( -16.84014894278199392, 407.6198905683720568, 11.84573899990672530 ) ) ;
#16873 = CARTESIAN_POINT ( 'NONE',  ( -10.20829729246300310, 511.6198905601785327, 7.653668647301790529 ) ) ;
#16874 = CARTESIAN_POINT ( 'NONE',  ( -48.68588794268871567, 396.9323905601785327, -3.978247347593158345 ) ) ;
#16875 = ORIENTED_EDGE ( 'NONE', *, *, #18846, .F. ) ;
#16876 = CARTESIAN_POINT ( 'NONE',  ( -4.646822748637091660E-15, 5.948846446048900560, -2.696295709017756614 ) ) ;
#16877 = ORIENTED_EDGE ( 'NONE', *, *, #17558, .F. ) ;
#16878 = VERTEX_POINT ( 'NONE', #10171 ) ;
#16879 = CARTESIAN_POINT ( 'NONE',  ( -11.93348319268874214, 530.0573905683720568, 3.332260488124728415 ) ) ;
#16880 = CARTESIAN_POINT ( 'NONE',  ( -36.33955658999050087, 285.3698905601784759, -18.47759065022572855 ) ) ;
#16881 = DIRECTION ( 'NONE',  ( 1.000000000000000000, 0.000000000000000000, 0.000000000000000000 ) ) ;
#16882 = CARTESIAN_POINT ( 'NONE',  ( -32.01814843081344009, 317.5573905683720568, 16.75240474999999307 ) ) ;
#16883 = ORIENTED_EDGE ( 'NONE', *, *, #107, .F. ) ;
#16884 = CARTESIAN_POINT ( 'NONE',  ( -13.20868407381886023, 368.2448905683720000, 6.410867750099229490 ) ) ;
#16885 = CARTESIAN_POINT ( 'NONE',  ( -19.19641293061498288, 370.4323905683719431, -14.20200298773971603 ) ) ;
#16886 = CARTESIAN_POINT ( 'NONE',  ( -14.54375231895776466, 308.2448905765656377, -14.14213562373094746 ) ) ;
#16887 = FACE_OUTER_BOUND ( 'NONE', #21074, .T. ) ;
#16888 = CARTESIAN_POINT ( 'NONE',  ( -19.19641293061496867, 267.3073905683720568, 14.20200298773971426 ) ) ;
#16889 = CARTESIAN_POINT ( 'NONE',  ( -21.03221929538692336, 465.1198905765655809, 18.47759065022572500 ) ) ;
#16890 = APPLICATION_CONTEXT ( 'automotive_design' ) ;
#16891 = ADVANCED_FACE ( 'NONE', ( #5408 ), #16686, .T. ) ;
#16892 = CARTESIAN_POINT ( 'NONE',  ( -25.35362745456399836, 412.5573905683719431, -16.75240474999999307 ) ) ;
#16893 = ADVANCED_FACE ( 'NONE', ( #13547, #15280, #13864 ), #8766, .T. ) ;
#16894 = DIRECTION ( 'NONE',  ( 0.000000000000000000, 0.000000000000000000, -1.000000000000000000 ) ) ;
#16895 = CARTESIAN_POINT ( 'NONE',  ( -11.73070664223724791, 353.1823905601785327, -11.32908994701042538 ) ) ;
#16896 = CARTESIAN_POINT ( 'NONE',  ( -17.35679799567828141, 305.4323905765655809, 16.95518130045146421 ) ) ;
#16897 = DIRECTION ( 'NONE',  ( 0.000000000000000000, 1.000000000000000000, 0.000000000000000000 ) ) ;
#16898 = CARTESIAN_POINT ( 'NONE',  ( -32.01814843081344009, 323.1823905683720000, -16.75240474999999307 ) ) ;
#16899 = CARTESIAN_POINT ( 'NONE',  ( -40.53162694259545162, 472.6198905683720000, -11.84573899990672707 ) ) ;
#16900 = VERTEX_POINT ( 'NONE', #20452 ) ;
#16901 = CARTESIAN_POINT ( 'NONE',  ( -45.64106924314020119, 466.3073905601785327, -11.32908994701042715 ) ) ;
#16902 = CARTESIAN_POINT ( 'NONE',  ( -28.68588794268870856, 291.3698905683720568, -16.75240474999999307 ) ) ;
#16903 = EDGE_CURVE ( 'NONE', #7992, #126, #3688, .T. ) ;
#16904 = CARTESIAN_POINT ( 'NONE',  ( -49.57497958038184294, -6.743947802724785386E-15, 0.000000000000000000 ) ) ;
#16905 = ORIENTED_EDGE ( 'NONE', *, *, #4468, .F. ) ;
#16906 = DIRECTION ( 'NONE',  ( -0.3512089204514979301, 0.000000000000000000, 0.9362971185447991340 ) ) ;
#16907 = CARTESIAN_POINT ( 'NONE',  ( -48.68588794268870856, 347.5573905601784759, 3.978247347593168115 ) ) ;
#16908 = EDGE_CURVE ( 'NONE', #11409, #12297, #13758, .T. ) ;
#16909 = CARTESIAN_POINT ( 'NONE',  ( -13.20868407381886200, 389.7448905683720000, 6.410867750099229490 ) ) ;
#16910 = CARTESIAN_POINT ( 'NONE',  ( -36.33955658999050087, 295.3698905601784759, -18.47759065022572855 ) ) ;
#16911 = CYLINDRICAL_SURFACE ( 'NONE', #5546, 19.99999999999999645 ) ;
#16912 = CARTESIAN_POINT ( 'NONE',  ( -13.20868407381886733, 419.4948905683720000, -6.410867750099233042 ) ) ;
#16913 = CARTESIAN_POINT ( 'NONE',  ( -35.09675569278793006, 263.4948905683720000, -15.47720386886985544 ) ) ;
#16914 = CARTESIAN_POINT ( 'NONE',  ( -14.48388495494900674, 417.9323905683720568, 9.489475012073731008 ) ) ;
#16915 = SHAPE_DEFINITION_REPRESENTATION ( #8199, #4076 ) ;
#16916 =( BOUNDED_CURVE ( )  B_SPLINE_CURVE ( 2, ( #20648, #12428, #4631, #19341, #9495, #15795, #14284, #17822, #19448, #4421, #11225, #16216, #17508, #12543, #7863, #17718, #982 ),
 .UNSPECIFIED., .F., .T. ) 
 B_SPLINE_CURVE_WITH_KNOTS ( ( 3, 2, 2, 2, 2, 2, 2, 2, 3 ),
 ( 0.4062500000000001665, 0.4082031250000001665, 0.4101562500000001665, 0.4121093750000001665, 0.4140625000000001665, 0.4160156250000001665, 0.4179687500000001665, 0.4199218750000001665, 0.4218750000000001665 ),
 .UNSPECIFIED. ) 
 CURVE ( )  GEOMETRIC_REPRESENTATION_ITEM ( )  RATIONAL_B_SPLINE_CURVE ( ( 0.9999999999999983347, 0.9807852804032320959, 1.000000000000000000, 0.9807852804032304306, 1.000000000000000000, 0.9807852804032304306, 1.000000000000000000, 0.9807852804032304306, 1.000000000000000000, 0.9807852804032304306, 1.000000000000000000, 0.9807852804032304306, 1.000000000000000000, 0.9807852804032304306, 1.000000000000000000, 0.9807852804032287652, 1.000000000000001554 ) ) 
 REPRESENTATION_ITEM ( '' )  );
#16917 = CARTESIAN_POINT ( 'NONE',  ( -28.68588794268871212, 354.4948905765656377, 19.99999999999999289 ) ) ;
#16918 = CARTESIAN_POINT ( 'NONE',  ( -36.33955658999050087, 275.3698905601784759, -18.47759065022572855 ) ) ;
#16919 = VECTOR ( 'NONE', #4483, 1000.000000000000000 ) ;
#16920 = CARTESIAN_POINT ( 'NONE',  ( -16.84014894278198682, 320.1198905683720568, -11.84573899990672707 ) ) ;
#16921 = CARTESIAN_POINT ( 'NONE',  ( -21.03221929538694113, 488.8698905765655809, -18.47759065022572855 ) ) ;
#16922 = CARTESIAN_POINT ( 'NONE',  ( -13.20868407381887089, 469.7448905683720568, 6.410867750099229490 ) ) ;
#16923 = EDGE_CURVE ( 'NONE', #18084, #21047, #252, .T. ) ;
#16924 = CARTESIAN_POINT ( 'NONE',  ( -45.64106924314018698, 432.9323905765656946, 11.32908994701042538 ) ) ;
#16925 = CARTESIAN_POINT ( 'NONE',  ( -43.64324723180579468, 200.2731091681331463, -1.141620385913092228 ) ) ;
#16926 = CARTESIAN_POINT ( 'NONE',  ( 30.42502041961813575, 271.1055109169419097, 20.00000000000000355 ) ) ;
#16927 = CIRCLE ( 'NONE', #3781, 4.000000000000003553 ) ;
#16928 = CARTESIAN_POINT ( 'NONE',  ( -14.48388495494900141, 389.4323905683720568, 9.489475012073732785 ) ) ;
#16929 = CARTESIAN_POINT ( 'NONE',  ( -48.68588794268873698, 573.2448905601785327, 0.000000000000000000 ) ) ;
#16930 = CARTESIAN_POINT ( 'NONE',  ( -36.33955658999053639, 529.1198905601785327, 18.47759065022572500 ) ) ;
#16931 = CARTESIAN_POINT ( 'NONE',  ( -35.09675569278795138, 355.7448905683720568, 15.47720386886985366 ) ) ;
#16932 = VERTEX_POINT ( 'NONE', #5518 ) ;
#16933 = CARTESIAN_POINT ( 'NONE',  ( -40.53162694259545873, 525.1198905683720568, 11.84573899990672885 ) ) ;
#16934 = ORIENTED_EDGE ( 'NONE', *, *, #20866, .F. ) ;
#16935 = CARTESIAN_POINT ( 'NONE',  ( -13.20868407381887799, 518.2448905683720568, 6.410867750099229490 ) ) ;
#16936 = ORIENTED_EDGE ( 'NONE', *, *, #17946, .F. ) ;
#16937 = CARTESIAN_POINT ( 'NONE',  ( -48.68588794268872988, 531.9948905765656946, 0.000000000000000000 ) ) ;
#16938 = CARTESIAN_POINT ( 'NONE',  ( -25.35362745456399480, 476.6823905683720000, 16.75240474999998952 ) ) ;
#16939 = ORIENTED_EDGE ( 'NONE', *, *, #12878, .F. ) ;
#16940 = CARTESIAN_POINT ( 'NONE',  ( -42.88789093042844769, 484.8073905683720000, 9.489475012073734561 ) ) ;
#16941 = DIRECTION ( 'NONE',  ( 0.000000000000000000, -1.000000000000000000, 0.000000000000000000 ) ) ;
#16942 = CARTESIAN_POINT ( 'NONE',  ( -47.16347859291445133, 431.3698905765655809, -7.653668647301793193 ) ) ;
#16943 = CARTESIAN_POINT ( 'NONE',  ( -48.68588794268885778, 472.3073905765656377, 3.978247347592849259 ) ) ;
#16944 = EDGE_CURVE ( 'NONE', #18782, #10157, #2678, .T. ) ;
#16945 = LINE ( 'NONE', #14025, #3712 ) ;
#16946 = DIRECTION ( 'NONE',  ( 0.000000000000000000, 1.000000000000000000, -0.000000000000000000 ) ) ;
#16947 = LINE ( 'NONE', #8709, #17707 ) ;
#16948 =( LENGTH_UNIT ( ) NAMED_UNIT ( * ) SI_UNIT ( .MILLI., .METRE. ) );
#16949 = DIRECTION ( 'NONE',  ( 0.000000000000000000, -0.5000000000000018874, -0.8660254037844375974 ) ) ;
#16950 = CARTESIAN_POINT ( 'NONE',  ( -28.68588794268870856, 302.8698905683720000, -16.75240474999999307 ) ) ;
#16951 = CYLINDRICAL_SURFACE ( 'NONE', #3003, 10.00000000000000888 ) ;
#16952 = CARTESIAN_POINT ( 'NONE',  ( -19.19641293061498999, 448.8073905683720568, 14.20200298773971426 ) ) ;
#16953 = DIRECTION ( 'NONE',  ( -0.9864615503757148129, 0.000000000000000000, 0.1639927121256942455 ) ) ;
#16954 = CARTESIAN_POINT ( 'NONE',  ( -14.48388495494898720, 269.4323905683720568, 9.489475012073732785 ) ) ;
#16955 = ORIENTED_EDGE ( 'NONE', *, *, #20481, .F. ) ;
#16956 = AXIS2_PLACEMENT_3D ( 'NONE', #11066, #3072, #8131 ) ;
#16957 = CARTESIAN_POINT ( 'NONE',  ( -42.82802356641964536, 268.4948905601784759, 14.14213562373094923 ) ) ;
#16958 = CARTESIAN_POINT ( 'NONE',  ( -25.35362745456400901, 502.5573905683720000, -16.75240474999999307 ) ) ;
#16959 = EDGE_CURVE ( 'NONE', #14497, #289, #12120, .T. ) ;
#16960 = AXIS2_PLACEMENT_3D ( 'NONE', #13936, #18887, #959 ) ;
#16961 = AXIS2_PLACEMENT_3D ( 'NONE', #9541, #3062, #6506 ) ;
#16962 = VERTEX_POINT ( 'NONE', #8653 ) ;
#16963 = CARTESIAN_POINT ( 'NONE',  ( -42.88789093042844769, 476.3073905683720000, 9.489475012073736337 ) ) ;
#16964 = DIRECTION ( 'NONE',  ( 0.000000000000000000, 0.000000000000000000, -1.000000000000000000 ) ) ;
#16965 = CARTESIAN_POINT ( 'NONE',  ( -45.43829269268869098, 253.5573905683720284, -3.332260488124726194 ) ) ;
#16966 = CIRCLE ( 'NONE', #7952, 22.72497359561857877 ) ;
#16967 = ORIENTED_EDGE ( 'NONE', *, *, #15811, .F. ) ;
#16968 = PLANE ( 'NONE',  #9709 ) ;
#16969 = CARTESIAN_POINT ( 'NONE',  ( -17.35679799567830983, 478.5573905765656377, -16.95518130045146421 ) ) ;
#16970 = CYLINDRICAL_SURFACE ( 'NONE', #13776, 19.99999999999999645 ) ;
#16971 = CARTESIAN_POINT ( 'NONE',  ( -40.53162694259542320, 244.1198905683720284, -11.84573899990672707 ) ) ;
#16972 = CARTESIAN_POINT ( 'NONE',  ( 158.8141120573112630, 400.5398297725602674, 0.000000000000000000 ) ) ;
#16973 = CARTESIAN_POINT ( 'NONE',  ( -28.68588794268869790, 224.7448905601784759, -19.99999999999999289 ) ) ;
#16974 = CARTESIAN_POINT ( 'NONE',  ( -32.01814843081343298, 251.6823905683720568, -16.75240474999999307 ) ) ;
#16975 = CARTESIAN_POINT ( 'NONE',  ( -42.88789093042843348, 364.4323905683720568, -9.489475012073736337 ) ) ;
#16976 = EDGE_CURVE ( 'NONE', #368, #18118, #12012, .T. ) ;
#16977 = CARTESIAN_POINT ( 'NONE',  ( 158.8141120573112630, 628.3356379279406383, 0.000000000000000000 ) ) ;
#16978 = AXIS2_PLACEMENT_3D ( 'NONE', #2091, #8672, #15296 ) ;
#16979 = AXIS2_PLACEMENT_3D ( 'NONE', #14881, #6633, #19843 ) ;
#16980 = CARTESIAN_POINT ( 'NONE',  ( -11.93348319268872615, 398.8698905683720000, -2.051577885510841163E-15 ) ) ;
#16981 = CARTESIAN_POINT ( 'NONE',  ( -21.03221929538691981, 338.8698905765656377, -18.47759065022572855 ) ) ;
#16982 = CARTESIAN_POINT ( 'NONE',  ( -42.82802356641966668, 405.9948905601785327, -14.14213562373094746 ) ) ;
#16983 = EDGE_CURVE ( 'NONE', #15984, #19418, #17471, .T. ) ;
#16984 = ORIENTED_EDGE ( 'NONE', *, *, #9663, .F. ) ;
#16985 = FACE_BOUND ( 'NONE', #19209, .T. ) ;
#16986 = ORIENTED_EDGE ( 'NONE', *, *, #14743, .F. ) ;
#16987 = ORIENTED_EDGE ( 'NONE', *, *, #9889, .T. ) ;
#16988 = CARTESIAN_POINT ( 'NONE',  ( -45.43829269268873361, 535.3698905683720568, 0.000000000000000000 ) ) ;
#16989 = CARTESIAN_POINT ( 'NONE',  ( -10.20829729246297646, 281.6198905601784759, 7.653668647301790529 ) ) ;
#16990 = CARTESIAN_POINT ( 'NONE',  ( -43.52372910701232911, 209.6355236139544331, -2.220491386914098531 ) ) ;
#16991 = CARTESIAN_POINT ( 'NONE',  ( -44.16309181155856578, 314.7448905683720000, -6.410867750099231266 ) ) ;
#16992 = PRESENTATION_LAYER_ASSIGNMENT (  '', '', ( #14239 ) ) ;
#16993 = VERTEX_POINT ( 'NONE', #2821 ) ;
#16994 = CARTESIAN_POINT ( 'NONE',  ( -22.27502019258948351, 340.7448905683720568, -15.47720386886985544 ) ) ;
#16995 = CARTESIAN_POINT ( 'NONE',  ( -45.43829269268871229, 374.1823905683720568, 3.332260488124734632 ) ) ;
#16996 = CARTESIAN_POINT ( 'NONE',  ( -45.64106924314017988, 292.9323905765656377, 11.32908994701042715 ) ) ;
#16997 = CARTESIAN_POINT ( 'NONE',  ( -46.31968306282883674, 135.1716627696692683, -33.59072564020502938 ) ) ;
#16998 = CARTESIAN_POINT ( 'NONE',  ( -45.43829269268869808, 263.8698905683720000, 0.000000000000000000 ) ) ;
#16999 = CARTESIAN_POINT ( 'NONE',  ( -48.68588794268872277, 461.9948905765656377, 0.000000000000000000 ) ) ;
#17000 = CARTESIAN_POINT ( 'NONE',  ( -11.93348319268872615, 410.6823905683720000, -3.332260488124732856 ) ) ;
#17001 = CARTESIAN_POINT ( 'NONE',  ( 28.16023193154655502, 323.8848358243226357, -20.00000000000000355 ) ) ;
#17002 = CARTESIAN_POINT ( 'NONE',  ( -17.35679799567830628, 505.4323905765656377, 16.95518130045146421 ) ) ;
#17003 = DIRECTION ( 'NONE',  ( -1.232945044042657126E-32, 9.855701800883825964E-17, 1.000000000000000000 ) ) ;
#17004 = CARTESIAN_POINT ( 'NONE',  ( -22.27502019258948351, 322.2448905683720000, -15.47720386886985544 ) ) ;
#17005 = CARTESIAN_POINT ( 'NONE',  ( -38.17536295476246977, 472.3073905683720568, -14.20200298773971426 ) ) ;
#17006 = ORIENTED_EDGE ( 'NONE', *, *, #15910, .T. ) ;
#17007 = AXIS2_PLACEMENT_3D ( 'NONE', #15652, #10540, #12286 ) ;
#17008 = CARTESIAN_POINT ( 'NONE',  ( -11.73070664223726389, 473.1823905601784190, -11.32908994701042715 ) ) ;
#17009 = CARTESIAN_POINT ( 'NONE',  ( -44.16309181155855867, 284.4948905683720000, 6.410867750099241924 ) ) ;
#17010 = ORIENTED_EDGE ( 'NONE', *, *, #13008, .T. ) ;
#17011 = PLANE ( 'NONE',  #20536 ) ;
#17012 = CARTESIAN_POINT ( 'NONE',  ( -48.68588794268870856, 336.9323905601784759, -3.978247347593158345 ) ) ;
#17013 = CARTESIAN_POINT ( 'NONE',  ( -40.53162694259543031, 302.6198905683720000, -11.84573899990672707 ) ) ;
#17014 = CARTESIAN_POINT ( 'NONE',  ( -19.19641293061498288, 388.8073905683720568, 14.20200298773971426 ) ) ;
#17015 = CARTESIAN_POINT ( 'NONE',  ( -48.68588794268870146, 297.2448905601784759, 0.000000000000000000 ) ) ;
#17016 = CARTESIAN_POINT ( 'NONE',  ( -24.70764059509558308, 519.1823905765655809, -19.99999999999999289 ) ) ;
#17017 = CARTESIAN_POINT ( 'NONE',  ( -35.09675569278795848, 405.7448905683720568, 15.47720386886985366 ) ) ;
#17018 = CARTESIAN_POINT ( 'NONE',  ( -16.84014894278197616, 269.1198905683720568, 11.84573899990672530 ) ) ;
#17019 = CIRCLE ( 'NONE', #6300, 9.999999999999980460 ) ;
#17020 = CARTESIAN_POINT ( 'NONE',  ( -25.35362745456398770, 416.6823905683720568, 16.75240474999998952 ) ) ;
#17021 = CARTESIAN_POINT ( 'NONE',  ( -47.16347859291444422, 372.6198905765655809, 7.653668647301805628 ) ) ;
#17022 = DIRECTION ( 'NONE',  ( -0.000000000000000000, 1.000000000000000000, -0.000000000000000000 ) ) ;
#17023 = CARTESIAN_POINT ( 'NONE',  ( -35.09675569278793716, 321.9948905683720568, -15.47720386886985544 ) ) ;
#17024 =( NAMED_UNIT ( * ) SI_UNIT ( $, .STERADIAN. ) SOLID_ANGLE_UNIT ( ) );
#17025 = CARTESIAN_POINT ( 'NONE',  ( -42.88789093042844769, 484.4323905683719431, -9.489475012073736337 ) ) ;
#17026 = ADVANCED_FACE ( 'NONE', ( #20985 ), #19253, .T. ) ;
#17027 = CARTESIAN_POINT ( 'NONE',  ( 20.42502041961813930, 230.5765313837437418, -49.99999999999999289 ) ) ;
#17028 = LINE ( 'NONE', #5544, #20773 ) ;
#17029 = LINE ( 'NONE', #8795, #1972 ) ;
#17030 = ADVANCED_FACE ( 'NONE', ( #2605 ), #619, .T. ) ;
#17031 = EDGE_CURVE ( 'NONE', #10415, #11766, #2499, .T. ) ;
#17032 = CARTESIAN_POINT ( 'NONE',  ( -11.93348319268872260, 380.3698905683720568, -2.051577885510841163E-15 ) ) ;
#17033 = CARTESIAN_POINT ( 'NONE',  ( -8.685887942688742314, 573.2448905601785327, 2.449293598294706119E-15 ) ) ;
#17034 = CARTESIAN_POINT ( 'NONE',  ( -8.685887942688740537, 522.2448905601784190, -2.449293598294705724E-15 ) ) ;
#17035 = CARTESIAN_POINT ( 'NONE',  ( -38.17536295476245556, 352.3073905683720000, -14.20200298773971426 ) ) ;
#17036 = EDGE_LOOP ( 'NONE', ( #12266, #230, #5142, #17119 ) ) ;
#17037 = CARTESIAN_POINT ( 'NONE',  ( -25.35362745456399836, 516.6823905683720568, 16.75240474999998952 ) ) ;
#17038 = EDGE_LOOP ( 'NONE', ( #18610, #10447, #2044, #6937 ) ) ;
#17039 =( BOUNDED_CURVE ( )  B_SPLINE_CURVE ( 2, ( #12270, #15636, #7281, #2433, #7388, #14015, #12163, #1216, #17249, #18750, #15528, #17040, #20594, #20494, #6165, #12051, #14418 ),
 .UNSPECIFIED., .F., .T. ) 
 B_SPLINE_CURVE_WITH_KNOTS ( ( 3, 2, 2, 2, 2, 2, 2, 2, 3 ),
 ( 0.4687500000000002220, 0.4707031250000002220, 0.4726562500000002220, 0.4746093750000002220, 0.4765625000000002220, 0.4785156250000002220, 0.4804687500000002220, 0.4824218750000002220, 0.4843750000000002220 ),
 .UNSPECIFIED. ) 
 CURVE ( )  GEOMETRIC_REPRESENTATION_ITEM ( )  RATIONAL_B_SPLINE_CURVE ( ( 0.9999999999999977796, 0.9807852804032326510, 1.000000000000000000, 0.9807852804032304306, 1.000000000000000000, 0.9807852804032304306, 1.000000000000000000, 0.9807852804032304306, 1.000000000000000000, 0.9807852804032304306, 1.000000000000000000, 0.9807852804032304306, 1.000000000000000000, 0.9807852804032304306, 1.000000000000000000, 0.9807852804032282101, 1.000000000000002220 ) ) 
 REPRESENTATION_ITEM ( '' )  );
#17040 = CARTESIAN_POINT ( 'NONE',  ( -17.35679799567829917, 378.5573905765656946, -16.95518130045146421 ) ) ;
#17041 = CARTESIAN_POINT ( 'NONE',  ( -22.30770786884143675, 45.31613216062291372, 122.9933582338429687 ) ) ;
#17042 = EDGE_CURVE ( 'NONE', #7286, #18039, #17211, .T. ) ;
#17043 = DIRECTION ( 'NONE',  ( 0.4627175328665443232, 5.514621922230504147E-17, -0.8865057725575725689 ) ) ;
#17044 = CARTESIAN_POINT ( 'NONE',  ( -32.66413529028188378, 495.0573905601784759, -19.99999999999999289 ) ) ;
#17045 = CARTESIAN_POINT ( 'NONE',  ( -38.17536295476246977, 492.3073905683720000, -14.20200298773971426 ) ) ;
#17046 = ORIENTED_EDGE ( 'NONE', *, *, #14236, .T. ) ;
#17047 = CARTESIAN_POINT ( 'NONE',  ( -45.43829269268872650, 493.5573905683720000, -3.332260488124726638 ) ) ;
#17048 = DIRECTION ( 'NONE',  ( -0.000000000000000000, -0.000000000000000000, 1.000000000000000000 ) ) ;
#17049 = CIRCLE ( 'NONE', #7701, 25.00000000000000711 ) ;
#17050 = CARTESIAN_POINT ( 'NONE',  ( -8.685887942688729879, 426.6823905765655809, 3.978247347593161010 ) ) ;
#17051 = PLANE ( 'NONE',  #9280 ) ;
#17052 = DIRECTION ( 'NONE',  ( 0.000000000000000000, 1.000000000000000000, 0.000000000000000000 ) ) ;
#17053 = CARTESIAN_POINT ( 'NONE',  ( 52.60622592008805043, 30.52886280891152282, 151.0302712373927250 ) ) ;
#17054 = CARTESIAN_POINT ( 'NONE',  ( -36.33955658999052929, 483.8698905765656377, 18.47759065022572500 ) ) ;
#17055 = DIRECTION ( 'NONE',  ( -1.000000000000000000, 0.000000000000000000, 0.000000000000000000 ) ) ;
#17056 = CARTESIAN_POINT ( 'NONE',  ( -11.73070664223725856, 433.1823905601784759, -11.32908994701042538 ) ) ;
#17057 = CARTESIAN_POINT ( 'NONE',  ( 0.06682554136338046680, -4.993536075455419443, 4.350941807883118351 ) ) ;
#17058 = CARTESIAN_POINT ( 'NONE',  ( -25.35362745456396993, 278.1823905683720000, 16.75240474999998952 ) ) ;
#17059 = CARTESIAN_POINT ( 'NONE',  ( -47.16347859291443001, 256.6198905601784759, -7.653668647301793193 ) ) ;
#17060 = CARTESIAN_POINT ( 'NONE',  ( -11.73070664223724968, 406.0573905765655240, 11.32908994701042005 ) ) ;
#17061 = CARTESIAN_POINT ( 'NONE',  ( -40.53162694259544452, 444.1198905683720568, -11.84573899990672707 ) ) ;
#17062 = CARTESIAN_POINT ( 'NONE',  ( -48.68588794268871567, 401.9948905765656377, 0.000000000000000000 ) ) ;
#17063 = CARTESIAN_POINT ( 'NONE',  ( -44.16309181155855867, 275.9948905683720000, 6.410867750099241924 ) ) ;
#17064 = VECTOR ( 'NONE', #13931, 1000.000000000000000 ) ;
#17065 = ORIENTED_EDGE ( 'NONE', *, *, #13854, .T. ) ;
#17066 = LINE ( 'NONE', #18245, #11522 ) ;
#17067 = CARTESIAN_POINT ( 'NONE',  ( -38.17536295476246266, 476.9323905683720568, 14.20200298773971781 ) ) ;
#17068 = AXIS2_PLACEMENT_3D ( 'NONE', #12656, #4433, #20743 ) ;
#17069 = ORIENTED_EDGE ( 'NONE', *, *, #9361, .T. ) ;
#17070 = CARTESIAN_POINT ( 'NONE',  ( 91.21585410611801592, 31.85652257517428865, -40.00000000000000000 ) ) ;
#17071 = CARTESIAN_POINT ( 'NONE',  ( -11.93348319268871194, 269.1823905683720000, -3.332260488124732856 ) ) ;
#17072 = ORIENTED_EDGE ( 'NONE', *, *, #9208, .T. ) ;
#17073 = DIRECTION ( 'NONE',  ( -1.000000000000000000, 0.000000000000000000, -0.000000000000000000 ) ) ;
#17074 = CARTESIAN_POINT ( 'NONE',  ( -14.54375231895778242, 485.7448905765656377, 14.14213562373094568 ) ) ;
#17075 = CARTESIAN_POINT ( 'NONE',  ( -48.68588794268887199, 387.5573905601784190, 3.978247347592742678 ) ) ;
#17076 = CARTESIAN_POINT ( 'NONE',  ( -35.09675569278793006, 243.4948905683720284, -15.47720386886985544 ) ) ;
#17077 = CARTESIAN_POINT ( 'NONE',  ( -13.20868407381887621, 509.7448905683720000, 6.410867750099229490 ) ) ;
#17078 = CARTESIAN_POINT ( 'NONE',  ( -11.73070664223724791, 376.0573905765655809, 11.32908994701042005 ) ) ;
#17079 = CARTESIAN_POINT ( 'NONE',  ( -40.53162694259542320, 252.6198905683720284, -11.84573899990672707 ) ) ;
#17080 = CIRCLE ( 'NONE', #17764, 175.0000000000000284 ) ;
#17081 = CARTESIAN_POINT ( 'NONE',  ( -25.35362745456399125, 352.5573905683720568, -16.75240474999999307 ) ) ;
#17082 = EDGE_CURVE ( 'NONE', #12542, #13817, #19953, .T. ) ;
#17083 = DIRECTION ( 'NONE',  ( 0.000000000000000000, -1.000000000000000000, 0.000000000000000000 ) ) ;
#17084 = CARTESIAN_POINT ( 'NONE',  ( -44.16309181155857289, 394.4948905683720000, 6.410867750099241924 ) ) ;
#17085 = EDGE_CURVE ( 'NONE', #5504, #5552, #4108, .T. ) ;
#17086 = PLANE ( 'NONE',  #12927 ) ;
#17087 = CARTESIAN_POINT ( 'NONE',  ( -36.33955658999051508, 405.3698905601785327, -18.47759065022572855 ) ) ;
#17088 = ORIENTED_EDGE ( 'NONE', *, *, #19149, .F. ) ;
#17089 = FACE_OUTER_BOUND ( 'NONE', #4235, .T. ) ;
#17090 = ORIENTED_EDGE ( 'NONE', *, *, #8743, .T. ) ;
#17091 = VERTEX_POINT ( 'NONE', #12234 ) ;
#17092 = CARTESIAN_POINT ( 'NONE',  ( -35.09675569278797269, 517.2448905683719431, 15.47720386886985366 ) ) ;
#17093 = CARTESIAN_POINT ( 'NONE',  ( -48.68588794268870146, 287.2448905601784759, 0.000000000000000000 ) ) ;
#17094 = DIRECTION ( 'NONE',  ( 0.000000000000000000, 0.000000000000000000, -1.000000000000000000 ) ) ;
#17095 = VERTEX_POINT ( 'NONE', #10591 ) ;
#17096 = B_SPLINE_CURVE_WITH_KNOTS ( 'NONE', 3,
 ( #367, #3389, #5214, #13445, #8345, #8453, #8559, #16800 ),
 .UNSPECIFIED., .F., .F.,
 ( 4, 2, 2, 4 ),
 ( 0.003797433802554463222, 0.004743183970586255238, 0.005688934138618048121, 0.007580434474681636489 ),
 .UNSPECIFIED. ) ;
#17097 = CARTESIAN_POINT ( 'NONE',  ( -14.48388495494899608, 331.3073905683720000, -9.489475012073734561 ) ) ;
#17098 = ORIENTED_EDGE ( 'NONE', *, *, #15442, .T. ) ;
#17099 = CARTESIAN_POINT ( 'NONE',  ( -40.53162694259543741, 345.1198905683720568, 11.84573899990672885 ) ) ;
#17100 = CARTESIAN_POINT ( 'NONE',  ( -38.17536295476244845, 365.4323905683720568, 14.20200298773971781 ) ) ;
#17101 = CARTESIAN_POINT ( 'NONE',  ( -32.66413529028186957, 284.1823905765655809, 19.99999999999999289 ) ) ;
#17102 = FACE_OUTER_BOUND ( 'NONE', #12245, .T. ) ;
#17103 = CARTESIAN_POINT ( 'NONE',  ( -42.88789093042841927, 264.8073905683721136, 9.489475012073734561 ) ) ;
#17104 = CARTESIAN_POINT ( 'NONE',  ( -48.68588794268869435, 227.2448905601785043, 0.000000000000000000 ) ) ;
#17105 = CARTESIAN_POINT ( 'NONE',  ( -45.43829269268871229, 425.0573905683720568, -3.332260488124726194 ) ) ;
#17106 = EDGE_CURVE ( 'NONE', #17559, #12194, #21319, .T. ) ;
#17107 = EDGE_CURVE ( 'NONE', #12773, #2298, #889, .T. ) ;
#17108 = CARTESIAN_POINT ( 'NONE',  ( 14.09825962131072785, 303.6587712403113528, 49.99999999999999289 ) ) ;
#17109 = CARTESIAN_POINT ( 'NONE',  ( -8.685887942688731655, 446.9948905765655809, -2.449293598294705724E-15 ) ) ;
#17110 = CARTESIAN_POINT ( 'NONE',  ( 4.700000000000000178, -3.752776749732576800, -6.499999999999999112 ) ) ;
#17111 = CARTESIAN_POINT ( 'NONE',  ( -16.84014894278198682, 321.6198905683720568, -11.84573899990672707 ) ) ;
#17112 = CARTESIAN_POINT ( 'NONE',  ( -16.84014894278200103, 460.1198905683720568, -11.84573899990672707 ) ) ;
#17113 = ORIENTED_EDGE ( 'NONE', *, *, #6050, .T. ) ;
#17114 = CARTESIAN_POINT ( 'NONE',  ( -21.03221929538693757, 474.1198905601784759, -18.47759065022572855 ) ) ;
#17115 = CARTESIAN_POINT ( 'NONE',  ( -42.88789093042842637, 284.8073905683720568, 9.489475012073736337 ) ) ;
#17116 = ORIENTED_EDGE ( 'NONE', *, *, #13966, .T. ) ;
#17117 = CARTESIAN_POINT ( 'NONE',  ( -42.82802356641965957, 338.4948905601785327, 14.14213562373094923 ) ) ;
#17118 = CARTESIAN_POINT ( 'NONE',  ( -14.48388495494901029, 441.3073905683721136, -9.489475012073734561 ) ) ;
#17119 = ORIENTED_EDGE ( 'NONE', *, *, #11993, .T. ) ;
#17120 = FACE_OUTER_BOUND ( 'NONE', #20668, .T. ) ;
#17121 = CARTESIAN_POINT ( 'NONE',  ( -32.01814843081344009, 291.6823905683720568, -16.75240474999999307 ) ) ;
#17122 = EDGE_CURVE ( 'NONE', #18169, #13, #15598, .T. ) ;
#17123 = CARTESIAN_POINT ( 'NONE',  ( -40.53162694259543741, 374.1198905683720000, -11.84573899990672707 ) ) ;
#17124 = DIRECTION ( 'NONE',  ( -1.191790137725560488E-16, 1.000000000000000000, -0.000000000000000000 ) ) ;
#17125 = CARTESIAN_POINT ( 'NONE',  ( -28.68588794268873698, 519.4948905765655809, -19.99999999999999289 ) ) ;
#17126 = CARTESIAN_POINT ( 'NONE',  ( -16.84014894278199037, 397.6198905683720568, 11.84573899990672530 ) ) ;
#17127 = CARTESIAN_POINT ( 'NONE',  ( -35.09675569278793716, 247.2448905683720000, 15.47720386886985366 ) ) ;
#17128 = CARTESIAN_POINT ( 'NONE',  ( -19.19641293061498644, 427.3073905683720568, 14.20200298773971426 ) ) ;
#17129 = ITEM_DEFINED_TRANSFORMATION ( 'NONE', 'NONE', #7606,  #12794 ) ;
#17130 = CARTESIAN_POINT ( 'NONE',  ( -45.64106924314018698, 351.0573905765656377, -11.32908994701042715 ) ) ;
#17131 = CARTESIAN_POINT ( 'NONE',  ( -48.68588794268870146, 277.2448905601784759, 0.000000000000000000 ) ) ;
#17132 = CARTESIAN_POINT ( 'NONE',  ( -16.84014894278198327, 317.6198905683720568, 11.84573899990672530 ) ) ;
#17133 = CARTESIAN_POINT ( 'NONE',  ( -42.88789093042844769, 474.4323905683721136, -9.489475012073736337 ) ) ;
#17134 = EDGE_CURVE ( 'NONE', #5669, #5772, #15911, .T. ) ;
#17135 = CARTESIAN_POINT ( 'NONE',  ( -5.502341142637708238, 600.7448905601785327, 7.573322868991241741 ) ) ;
#17136 = CARTESIAN_POINT ( 'NONE',  ( 44.98449999999999704, 0.000000000000000000, 4.000000000000000000 ) ) ;
#17137 = CARTESIAN_POINT ( 'NONE',  ( -32.39665892562713623, 224.2034014279912526, 19.99999999999999289 ) ) ;
#17138 = CARTESIAN_POINT ( 'NONE',  ( -45.43829269268871229, 395.6823905683719431, 3.332260488124734632 ) ) ;
#17139 = CARTESIAN_POINT ( 'NONE',  ( -32.80098538532548957, 52.03835429381459221, -120.6197264542505536 ) ) ;
#17140 = CARTESIAN_POINT ( 'NONE',  ( -40.01497788969916058, 525.6823905601785327, -16.95518130045146421 ) ) ;
#17141 = CARTESIAN_POINT ( 'NONE',  ( -44.16309181155857289, 343.2448905683720000, -6.410867750099231266 ) ) ;
#17142 = EDGE_LOOP ( 'NONE', ( #4702, #15899, #4340, #20567 ) ) ;
#17143 = CARTESIAN_POINT ( 'NONE',  ( -13.20868407381887621, 498.2448905683720000, 6.410867750099229490 ) ) ;
#17144 = ORIENTED_EDGE ( 'NONE', *, *, #6057, .T. ) ;
#17145 = CARTESIAN_POINT ( 'NONE',  ( -10.20829729246299244, 417.6198905765656377, -7.653668647301794969 ) ) ;
#17146 = LINE ( 'NONE', #10524, #3238 ) ;
#17147 = CARTESIAN_POINT ( 'NONE',  ( -45.64106924314017277, 291.0573905765656377, -11.32908994701042538 ) ) ;
#17148 = CARTESIAN_POINT ( 'NONE',  ( 0.000000000000000000, -343.0245277843623057, 0.000000000000000000 ) ) ;
#17149 = CARTESIAN_POINT ( 'NONE',  ( -38.17536295476246266, 455.4323905683720000, 14.20200298773971781 ) ) ;
#17150 = ORIENTED_EDGE ( 'NONE', *, *, #9223, .F. ) ;
#17151 = CARTESIAN_POINT ( 'NONE',  ( -28.68588794268872988, 481.3698905683720568, -16.75240474999999307 ) ) ;
#17152 = CARTESIAN_POINT ( 'NONE',  ( -40.01497788969911795, 243.5573905765656377, 16.95518130045146776 ) ) ;
#17153 = CARTESIAN_POINT ( 'NONE',  ( -28.68588794268871922, 404.4948905765656377, 19.99999999999999289 ) ) ;
#17154 = CARTESIAN_POINT ( 'NONE',  ( 35.96497763894179656, 191.2380552923725645, -48.74187950074039577 ) ) ;
#17155 = CARTESIAN_POINT ( 'NONE',  ( 118.4271928232701043, -343.0245277843623057, -40.00000000000000000 ) ) ;
#17156 = CARTESIAN_POINT ( 'NONE',  ( -28.68588794268875120, 585.7448905601785327, 0.000000000000000000 ) ) ;
#17157 = DIRECTION ( 'NONE',  ( 0.000000000000000000, 0.000000000000000000, 1.000000000000000000 ) ) ;
#17158 = VECTOR ( 'NONE', #13255, 1000.000000000000000 ) ;
#17159 = CARTESIAN_POINT ( 'NONE',  ( -21.03221929538691271, 258.8698905765656377, -18.47759065022572855 ) ) ;
#17160 = CARTESIAN_POINT ( 'NONE',  ( -22.30770786884136214, -343.0245277843623057, 122.9933582338429972 ) ) ;
#17161 = ADVANCED_FACE ( 'NONE', ( #7453 ), #9581, .T. ) ;
#17162 = CARTESIAN_POINT ( 'NONE',  ( -13.20868407381884957, 270.9948905683720000, -6.410867750099233042 ) ) ;
#17163 = EDGE_CURVE ( 'NONE', #10333, #4398, #20664, .T. ) ;
#17164 = CARTESIAN_POINT ( 'NONE',  ( -28.68588794268870146, 254.7448905601784475, -19.99999999999999289 ) ) ;
#17165 = AXIS2_PLACEMENT_3D ( 'NONE', #14138, #12508, #5898 ) ;
#17166 = CARTESIAN_POINT ( 'NONE',  ( -48.68588794268870856, 361.9948905765655809, 0.000000000000000000 ) ) ;
#17167 = CARTESIAN_POINT ( 'NONE',  ( -25.35362745456399125, 438.1823905683720000, 16.75240474999998952 ) ) ;
#17168 = DIRECTION ( 'NONE',  ( 0.000000000000000000, 0.000000000000000000, -1.000000000000000000 ) ) ;
#17169 =( BOUNDED_CURVE ( )  B_SPLINE_CURVE ( 2, ( #1455, #6624, #8569, #8243, #5118, #15088, #11823, #15191, #14979, #1673, #13245, #11500, #18418, #11609, #11718, #6947, #13569 ),
 .UNSPECIFIED., .F., .T. ) 
 B_SPLINE_CURVE_WITH_KNOTS ( ( 3, 2, 2, 2, 2, 2, 2, 2, 3 ),
 ( 0.4218750000000001665, 0.4238281250000001665, 0.4257812500000001665, 0.4277343750000001665, 0.4296875000000002220, 0.4316406250000002220, 0.4335937500000002220, 0.4355468750000002220, 0.4375000000000002220 ),
 .UNSPECIFIED. ) 
 CURVE ( )  GEOMETRIC_REPRESENTATION_ITEM ( )  RATIONAL_B_SPLINE_CURVE ( ( 0.9999999999999983347, 0.9807852804032320959, 1.000000000000000000, 0.9807852804032304306, 1.000000000000000000, 0.9807852804032304306, 1.000000000000000000, 0.9807852804032304306, 1.000000000000000000, 0.9807852804032304306, 1.000000000000000000, 0.9807852804032304306, 1.000000000000000000, 0.9807852804032304306, 1.000000000000000000, 0.9807852804032282101, 1.000000000000002220 ) ) 
 REPRESENTATION_ITEM ( '' )  );
#17170 = CARTESIAN_POINT ( 'NONE',  ( -45.43829269268869808, 275.6823905683720568, 3.332260488124734632 ) ) ;
#17171 = ORIENTED_EDGE ( 'NONE', *, *, #1000, .F. ) ;
#17172 = ORIENTED_EDGE ( 'NONE', *, *, #6348, .T. ) ;
#17173 = CARTESIAN_POINT ( 'NONE',  ( -11.93348319268873681, 490.0573905683720568, 3.332260488124728859 ) ) ;
#17174 = VECTOR ( 'NONE', #16953, 1000.000000000000114 ) ;
#17175 = ORIENTED_EDGE ( 'NONE', *, *, #21383, .T. ) ;
#17176 = CARTESIAN_POINT ( 'NONE',  ( -5.502341142637706461, 585.7448905601785327, 7.573322868991241741 ) ) ;
#17177 = CARTESIAN_POINT ( 'NONE',  ( -42.88789093042841927, 244.8073905683720568, 9.489475012073736337 ) ) ;
#17178 = ORIENTED_EDGE ( 'NONE', *, *, #8344, .T. ) ;
#17179 = CARTESIAN_POINT ( 'NONE',  ( -31.26501780185373391, 205.1437886375728965, 5.000000000000001776 ) ) ;
#17180 = AXIS2_PLACEMENT_3D ( 'NONE', #3404, #17888, #8139 ) ;
#17181 = CARTESIAN_POINT ( 'NONE',  ( -36.33955658999052218, 480.1198905765656377, -18.47759065022572855 ) ) ;
#17182 = CARTESIAN_POINT ( 'NONE',  ( -10.20829729246298001, 307.6198905765656377, -7.653668647301794969 ) ) ;
#17183 = CARTESIAN_POINT ( 'NONE',  ( -22.14532378356892295, 223.9102039777116318, -18.39083598434388733 ) ) ;
#17184 = CARTESIAN_POINT ( 'NONE',  ( -32.01814843081343298, 227.5573905683720284, 16.75240474999999307 ) ) ;
#17185 = CARTESIAN_POINT ( 'NONE',  ( -16.84014894278200458, 519.1198905683720568, 11.84573899990672530 ) ) ;
#17186 = CARTESIAN_POINT ( 'NONE',  ( 0.1061556211655339810, 6.421950209808280796, 1.876855952934450622 ) ) ;
#17187 = CARTESIAN_POINT ( 'NONE',  ( -45.43829269268869808, 243.8698905683720568, 0.000000000000000000 ) ) ;
#17188 = CARTESIAN_POINT ( 'NONE',  ( -35.09675569278794427, 343.4948905683720000, -15.47720386886985544 ) ) ;
#17189 = AXIS2_PLACEMENT_3D ( 'NONE', #2234, #17052, #15538 ) ;
#17190 = LINE ( 'NONE', #2475, #18520 ) ;
#17191 = VECTOR ( 'NONE', #14300, 1000.000000000000000 ) ;
#17192 = CARTESIAN_POINT ( 'NONE',  ( -45.43829269268871940, 393.8698905683720000, 0.000000000000000000 ) ) ;
#17193 = CARTESIAN_POINT ( 'NONE',  ( 51.50493485826542184, 141.8799693780962912, 94.99999999999994316 ) ) ;
#17194 = CARTESIAN_POINT ( 'NONE',  ( -28.68588794268871567, 379.7448905601785327, 19.99999999999999289 ) ) ;
#17195 = VERTEX_POINT ( 'NONE', #7562 ) ;
#17196 = CARTESIAN_POINT ( 'NONE',  ( -48.68588794268870856, 351.9948905765656377, 0.000000000000000000 ) ) ;
#17197 = ORIENTED_EDGE ( 'NONE', *, *, #13122, .T. ) ;
#17198 = ORIENTED_EDGE ( 'NONE', *, *, #13398, .T. ) ;
#17199 = CARTESIAN_POINT ( 'NONE',  ( -25.35362745456399836, 508.1823905683720568, 16.75240474999998952 ) ) ;
#17200 = CARTESIAN_POINT ( 'NONE',  ( -48.68588794268870146, 311.9948905765655809, 0.000000000000000000 ) ) ;
#17201 = ORIENTED_EDGE ( 'NONE', *, *, #63, .T. ) ;
#17202 = CARTESIAN_POINT ( 'NONE',  ( -44.16309181155855867, 305.9948905683720568, 6.410867750099241924 ) ) ;
#17203 = EDGE_LOOP ( 'NONE', ( #6783, #16011, #16939, #5848, #7201 ) ) ;
#17204 = CARTESIAN_POINT ( 'NONE',  ( -42.88789093042843348, 352.9323905683721136, -9.489475012073736337 ) ) ;
#17205 = CARTESIAN_POINT ( 'NONE',  ( -16.84014894278199037, 350.1198905683720568, -11.84573899990672707 ) ) ;
#17206 = CARTESIAN_POINT ( 'NONE',  ( -47.16347859291443712, 281.3698905765656377, -7.653668647301793193 ) ) ;
#17207 = DIRECTION ( 'NONE',  ( -1.191790137725560488E-16, 1.000000000000000000, -0.000000000000000000 ) ) ;
#17208 = CARTESIAN_POINT ( 'NONE',  ( -45.43829269268869808, 253.8698905683720000, 0.000000000000000000 ) ) ;
#17209 = CARTESIAN_POINT ( 'NONE',  ( -48.68588794268887909, 462.3073905765656377, 3.978247347592795524 ) ) ;
#17210 = CARTESIAN_POINT ( 'NONE',  ( -16.84014894278199392, 391.6198905683720568, -11.84573899990672707 ) ) ;
#17211 = LINE ( 'NONE', #7774, #17191 ) ;
#17212 = PRODUCT_DEFINITION_CONTEXT ( 'detailed design', #4184, 'design' ) ;
#17213 = CARTESIAN_POINT ( 'NONE',  ( -28.68588794268873698, 548.2448905601784190, 0.000000000000000000 ) ) ;
#17214 = CARTESIAN_POINT ( 'NONE',  ( -44.16309181155856578, 304.7448905683720568, -6.410867750099231266 ) ) ;
#17215 = CARTESIAN_POINT ( 'NONE',  ( -19.19641293061499354, 467.3073905683721136, 14.20200298773971426 ) ) ;
#17216 = ORIENTED_EDGE ( 'NONE', *, *, #7274, .F. ) ;
#17217 = CARTESIAN_POINT ( 'NONE',  ( -21.03221929538691981, 460.3698905601784759, 18.47759065022572500 ) ) ;
#17218 = CARTESIAN_POINT ( 'NONE',  ( -38.17536295476244845, 282.3073905683720568, -14.20200298773971426 ) ) ;
#17219 = ORIENTED_EDGE ( 'NONE', *, *, #17488, .F. ) ;
#17220 = CARTESIAN_POINT ( 'NONE',  ( -71.26501780185373036, 326.0737056351150613, 25.00000000000000355 ) ) ;
#17221 = ORIENTED_EDGE ( 'NONE', *, *, #9677, .T. ) ;
#17222 = EDGE_LOOP ( 'NONE', ( #5162, #19788, #16241, #13585 ) ) ;
#17223 = DIRECTION ( 'NONE',  ( -0.7071067811865530128, 0.000000000000000000, 0.7071067811865421326 ) ) ;
#17224 = CARTESIAN_POINT ( 'NONE',  ( -24.70764059509555821, 344.4323905601784759, -19.99999999999999289 ) ) ;
#17225 = CARTESIAN_POINT ( 'NONE',  ( -45.43829269268870519, 303.8698905683720000, 0.000000000000000000 ) ) ;
#17226 = EDGE_CURVE ( 'NONE', #6220, #8661, #11988, .T. ) ;
#17227 = CARTESIAN_POINT ( 'NONE',  ( -44.16309181155856578, 385.9948905683720568, 6.410867750099241924 ) ) ;
#17228 = CARTESIAN_POINT ( 'NONE',  ( -32.66413529028186957, 375.0573905601784759, -19.99999999999999289 ) ) ;
#17229 = CARTESIAN_POINT ( 'NONE',  ( -8.685887942688742314, 517.3073905765655809, -3.978247347593165895 ) ) ;
#17230 = CARTESIAN_POINT ( 'NONE',  ( -45.43829269268871229, 413.5573905683720000, -3.332260488124726194 ) ) ;
#17231 = CARTESIAN_POINT ( 'NONE',  ( -16.84014894278197616, 241.6198905683720284, -11.84573899990672707 ) ) ;
#17232 = CARTESIAN_POINT ( 'NONE',  ( -16.84014894278199392, 407.6198905683720568, 11.84573899990672530 ) ) ;
#17233 = CARTESIAN_POINT ( 'NONE',  ( -24.70764059509555821, 339.1823905765656377, -19.99999999999999289 ) ) ;
#17234 = LINE ( 'NONE', #20580, #4801 ) ;
#17235 = CARTESIAN_POINT ( 'NONE',  ( -22.27502019258947996, 300.7448905683720568, -15.47720386886985544 ) ) ;
#17236 = CARTESIAN_POINT ( 'NONE',  ( -44.16309181155858710, 474.7448905683720568, -6.410867750099231266 ) ) ;
#17237 = DIRECTION ( 'NONE',  ( 1.000000000000000000, 0.000000000000000000, 0.000000000000000000 ) ) ;
#17238 = DIRECTION ( 'NONE',  ( 0.000000000000000000, -0.5000000000000008882, 0.8660254037844381525 ) ) ;
#17239 = CARTESIAN_POINT ( 'NONE',  ( -8.685887942688715668, 302.2448905601784190, -2.449293598294705724E-15 ) ) ;
#17240 = EDGE_CURVE ( 'NONE', #12430, #9807, #5784, .T. ) ;
#17241 = CARTESIAN_POINT ( 'NONE',  ( -14.48388495494900496, 391.3073905683720000, -9.489475012073736337 ) ) ;
#17242 = DIRECTION ( 'NONE',  ( 0.000000000000000000, 0.000000000000000000, 1.000000000000000000 ) ) ;
#17243 = CARTESIAN_POINT ( 'NONE',  ( -17.35679799567830983, 520.6823905601785327, 16.95518130045146421 ) ) ;
#17244 = CARTESIAN_POINT ( 'NONE',  ( -11.93348319268872260, 349.1823905683720000, -3.332260488124732856 ) ) ;
#17245 = CONICAL_SURFACE ( 'NONE', #17579, 6.500000000000000000, 1.047197551196600296 ) ;
#17246 = ORIENTED_EDGE ( 'NONE', *, *, #11811, .T. ) ;
#17247 = CARTESIAN_POINT ( 'NONE',  ( -40.53162694259545873, 512.6198905683720568, -11.84573899990672707 ) ) ;
#17248 = ORIENTED_EDGE ( 'NONE', *, *, #8963, .F. ) ;
#17249 = CARTESIAN_POINT ( 'NONE',  ( -28.68588794268871922, 379.4948905765656377, -19.99999999999999289 ) ) ;
#17250 = CARTESIAN_POINT ( 'NONE',  ( -8.685887942688717445, 316.9948905765655809, -2.449293598294705724E-15 ) ) ;
#17251 = EDGE_CURVE ( 'NONE', #16862, #15664, #19252, .T. ) ;
#17252 = CARTESIAN_POINT ( 'NONE',  ( -28.68588794268869790, 223.9102039777116602, 0.000000000000000000 ) ) ;
#17253 = CARTESIAN_POINT ( 'NONE',  ( -32.66413529028189089, 519.8073905765655809, -19.99999999999999289 ) ) ;
#17254 = CARTESIAN_POINT ( 'NONE',  ( -11.93348319268873503, 468.5573905683720000, 3.332260488124728415 ) ) ;
#17255 = ORIENTED_EDGE ( 'NONE', *, *, #8497, .F. ) ;
#17256 = CARTESIAN_POINT ( 'NONE',  ( -22.27502019258949062, 476.9948905683720000, 15.47720386886985189 ) ) ;
#17257 = CARTESIAN_POINT ( 'NONE',  ( -32.66413529028185536, 249.4323905601784759, 19.99999999999999289 ) ) ;
#17258 = CARTESIAN_POINT ( 'NONE',  ( -21.03221929538691271, 395.1198905765656377, 18.47759065022572500 ) ) ;
#17259 = CARTESIAN_POINT ( 'NONE',  ( -28.68588794268875120, 585.7448905601785327, 0.000000000000000000 ) ) ;
#17260 = DIRECTION ( 'NONE',  ( 0.000000000000000000, 1.000000000000000000, 0.000000000000000000 ) ) ;
#17261 = CARTESIAN_POINT ( 'NONE',  ( 0.5805565836007597902, 3.752776749732560368, -6.499999999999999112 ) ) ;
#17262 = CYLINDRICAL_SURFACE ( 'NONE', #11133, 19.99999999999999645 ) ;
#17263 = DIRECTION ( 'NONE',  ( 1.191790137725560488E-16, -1.000000000000000000, -0.000000000000000000 ) ) ;
#17264 = FACE_BOUND ( 'NONE', #10024, .T. ) ;
#17265 = CARTESIAN_POINT ( 'NONE',  ( 30.42502041961813575, 271.1055109169419097, -20.00000000000000355 ) ) ;
#17266 = CARTESIAN_POINT ( 'NONE',  ( -35.09675569278793716, 283.4948905683720000, -15.47720386886985544 ) ) ;
#17267 = CARTESIAN_POINT ( 'NONE',  ( -40.01497788969912506, 245.6823905601784759, -16.95518130045146421 ) ) ;
#17268 = CARTESIAN_POINT ( 'NONE',  ( -48.68588794268885067, 402.3073905765656377, 3.978247347592849259 ) ) ;
#17269 = B_SPLINE_CURVE_WITH_KNOTS ( 'NONE', 3,
 ( #1387, #4415, #17607, #2798, #9384, #6135 ),
 .UNSPECIFIED., .F., .F.,
 ( 4, 2, 4 ),
 ( 0.01067228060976418112, 0.01257272967502433281, 0.01447317874028448276 ),
 .UNSPECIFIED. ) ;
#17270 = CARTESIAN_POINT ( 'NONE',  ( -32.01814843081345430, 443.1823905683720568, -16.75240474999999307 ) ) ;
#17271 = CARTESIAN_POINT ( 'NONE',  ( -8.685887942688541585, 327.3073905765655240, -3.978247347592740013 ) ) ;
#17272 = CARTESIAN_POINT ( 'NONE',  ( -22.27502019258946575, 268.4948905683720000, 15.47720386886985189 ) ) ;
#17273 = ORIENTED_EDGE ( 'NONE', *, *, #2898, .T. ) ;
#17274 = ORIENTED_EDGE ( 'NONE', *, *, #10616, .F. ) ;
#17275 = CARTESIAN_POINT ( 'NONE',  ( -16.84014894278200103, 489.1198905683720000, 11.84573899990672530 ) ) ;
#17276 = EDGE_LOOP ( 'NONE', ( #18714, #16032, #10425, #17274, #2020 ) ) ;
#17277 = CARTESIAN_POINT ( 'NONE',  ( -28.68588794268871567, 364.7448905601784759, -19.99999999999999289 ) ) ;
#17278 = CARTESIAN_POINT ( 'NONE',  ( -35.09675569278793006, 241.9948905683720284, -15.47720386886985544 ) ) ;
#17279 = ADVANCED_FACE ( 'NONE', ( #4851 ), #19464, .F. ) ;
#17280 = ORIENTED_EDGE ( 'NONE', *, *, #20876, .T. ) ;
#17281 = FACE_OUTER_BOUND ( 'NONE', #19474, .T. ) ;
#17282 = CARTESIAN_POINT ( 'NONE',  ( -47.16347859291445843, 471.3698905765656377, -7.653668647301793193 ) ) ;
#17283 = CARTESIAN_POINT ( 'NONE',  ( 51.50493485826542184, 160.1716627696692683, -61.61851857202071159 ) ) ;
#17284 = AXIS2_PLACEMENT_3D ( 'NONE', #8909, #15422, #9231 ) ;
#17285 = CARTESIAN_POINT ( 'NONE',  ( -8.685887942688731655, 452.2448905601784759, -2.449293598294705724E-15 ) ) ;
#17286 = CARTESIAN_POINT ( 'NONE',  ( -14.48388495494898187, 229.4323905683720000, 9.489475012073731008 ) ) ;
#17287 = CARTESIAN_POINT ( 'NONE',  ( -45.43829269268872650, 525.6823905683719431, 3.332260488124734632 ) ) ;
#17288 = CARTESIAN_POINT ( 'NONE',  ( -32.01814843081343298, 241.6823905683720568, -16.75240474999999307 ) ) ;
#17289 = CARTESIAN_POINT ( 'NONE',  ( -45.43829269268870519, 345.0573905683720568, -3.332260488124726194 ) ) ;
#17290 = EDGE_CURVE ( 'NONE', #10000, #21098, #4646, .T. ) ;
#17291 = CARTESIAN_POINT ( 'NONE',  ( -17.35679799567828496, 320.6823905601784190, 16.95518130045146421 ) ) ;
#17292 = CARTESIAN_POINT ( 'NONE',  ( -14.54375231895775933, 305.7448905765656377, 14.14213562373094568 ) ) ;
#17293 = EDGE_CURVE ( 'NONE', #3575, #4551, #8087, .T. ) ;
#17294 = ADVANCED_FACE ( 'NONE', ( #19779 ), #1305, .T. ) ;
#17295 = COLOUR_RGB ( '',0.7921568627450980005, 0.8196078431372548767, 0.9333333333333333481 ) ;
#17296 = CARTESIAN_POINT ( 'NONE',  ( -40.53162694259543741, 375.1198905683720000, 11.84573899990672885 ) ) ;
#17297 = CARTESIAN_POINT ( 'NONE',  ( -42.82802356641965957, 388.4948905601784759, 14.14213562373094923 ) ) ;
#17298 = CARTESIAN_POINT ( 'NONE',  ( -28.68588794268872633, 333.8848358243226357, 0.000000000000000000 ) ) ;
#17299 = ORIENTED_EDGE ( 'NONE', *, *, #20112, .T. ) ;
#17300 = ORIENTED_EDGE ( 'NONE', *, *, #7946, .F. ) ;
#17301 = CARTESIAN_POINT ( 'NONE',  ( -16.84014894278200458, 509.1198905683720568, 11.84573899990672530 ) ) ;
#17302 = DIRECTION ( 'NONE',  ( 1.000000000000000000, 0.000000000000000000, -0.000000000000000000 ) ) ;
#17303 = ORIENTED_EDGE ( 'NONE', *, *, #11824, .T. ) ;
#17304 = EDGE_CURVE ( 'NONE', #18961, #5934, #18215, .T. ) ;
#17305 = CARTESIAN_POINT ( 'NONE',  ( -11.93348319268871371, 300.3698905683720568, -2.051577885510841163E-15 ) ) ;
#17306 = ORIENTED_EDGE ( 'NONE', *, *, #18262, .F. ) ;
#17307 = CARTESIAN_POINT ( 'NONE',  ( -45.43829269268871229, 353.8698905683720568, 0.000000000000000000 ) ) ;
#17308 = CARTESIAN_POINT ( 'NONE',  ( -45.43829269268871229, 344.1823905683719431, 3.332260488124734632 ) ) ;
#17309 =( GEOMETRIC_REPRESENTATION_CONTEXT ( 3 ) GLOBAL_UNCERTAINTY_ASSIGNED_CONTEXT ( ( #16554 ) ) GLOBAL_UNIT_ASSIGNED_CONTEXT ( ( #1343, #13129, #11278 ) ) REPRESENTATION_CONTEXT ( 'NONE', 'WORKASPACE' ) );
#17310 = CARTESIAN_POINT ( 'NONE',  ( -45.64106924314017988, 282.9323905765656377, 11.32908994701042715 ) ) ;
#17311 = AXIS2_PLACEMENT_3D ( 'NONE', #13200, #1516, #11449 ) ;
#17312 = CARTESIAN_POINT ( 'NONE',  ( -45.64106924314018698, 396.3073905601784759, -11.32908994701042538 ) ) ;
#17313 = CARTESIAN_POINT ( 'NONE',  ( -14.48388495494898542, 239.8073905683720284, -9.489475012073734561 ) ) ;
#17314 = CARTESIAN_POINT ( 'NONE',  ( -42.82802356641964536, 205.1437886375728965, 5.000000000000001776 ) ) ;
#17315 = CARTESIAN_POINT ( 'NONE',  ( -35.09675569278795848, 397.2448905683720568, 15.47720386886985366 ) ) ;
#17316 = DIRECTION ( 'NONE',  ( 0.000000000000000000, 0.000000000000000000, 1.000000000000000000 ) ) ;
#17317 = CARTESIAN_POINT ( 'NONE',  ( -42.82802356641968089, 503.2448905765656377, 14.14213562373094923 ) ) ;
#17318 = CARTESIAN_POINT ( 'NONE',  ( -40.01497788969912506, 245.6823905601784759, -16.95518130045146421 ) ) ;
#17319 = CARTESIAN_POINT ( 'NONE',  ( -14.48388495494900674, 447.9323905683720000, 9.489475012073732785 ) ) ;
#17320 = VERTEX_POINT ( 'NONE', #14824 ) ;
#17321 = CARTESIAN_POINT ( 'NONE',  ( -28.68588794268872633, 454.7448905601784759, -19.99999999999999289 ) ) ;
#17322 = ORIENTED_EDGE ( 'NONE', *, *, #19528, .T. ) ;
#17323 = CARTESIAN_POINT ( 'NONE',  ( 0.000000000000000000, 0.000000000000000000, 4.000000000000000000 ) ) ;
#17324 = ORIENTED_EDGE ( 'NONE', *, *, #15983, .T. ) ;
#17325 = EDGE_LOOP ( 'NONE', ( #19822, #341, #19185 ) ) ;
#17326 = CARTESIAN_POINT ( 'NONE',  ( 0.5805565836007647862, -3.752776749732576356, -6.500000000000000000 ) ) ;
#17327 = AXIS2_PLACEMENT_3D ( 'NONE', #7765, #20976, #6144 ) ;
#17328 = CARTESIAN_POINT ( 'NONE',  ( -42.82802356641965247, 328.4948905601784759, 14.14213562373094923 ) ) ;
#17329 = CARTESIAN_POINT ( 'NONE',  ( -32.01814843081344009, 296.0573905683720000, 16.75240474999999307 ) ) ;
#17330 = CARTESIAN_POINT ( 'NONE',  ( -16.84014894278199037, 361.6198905683720000, -11.84573899990672707 ) ) ;
#17331 = LINE ( 'NONE', #2514, #1410 ) ;
#17332 = CARTESIAN_POINT ( 'NONE',  ( -24.70764059509557242, 524.8073905765655809, 19.99999999999998934 ) ) ;
#17333 = CARTESIAN_POINT ( 'NONE',  ( -16.84014894278199748, 410.1198905683720000, -11.84573899990672707 ) ) ;
#17334 = CARTESIAN_POINT ( 'NONE',  ( -32.01814843081343298, 243.1823905683720568, -16.75240474999999307 ) ) ;
#17335 = CARTESIAN_POINT ( 'NONE',  ( -35.09675569278795848, 405.7448905683720568, 15.47720386886985366 ) ) ;
#17336 = CARTESIAN_POINT ( 'NONE',  ( -42.82802356641965957, 343.2448905765656377, 14.14213562373094923 ) ) ;
#17337 = CARTESIAN_POINT ( 'NONE',  ( -42.82802356641965247, 325.9948905601784759, -14.14213562373094746 ) ) ;
#17338 = CARTESIAN_POINT ( 'NONE',  ( -32.01814843081344009, 311.6823905683720568, -16.75240474999999307 ) ) ;
#17339 = CARTESIAN_POINT ( 'NONE',  ( -40.53162694259545162, 456.6198905683720568, 11.84573899990672885 ) ) ;
#17340 = DIRECTION ( 'NONE',  ( 0.3090169943749473958, 0.000000000000000000, 0.9510565162951535312 ) ) ;
#17341 = FACE_OUTER_BOUND ( 'NONE', #4652, .T. ) ;
#17342 = FACE_OUTER_BOUND ( 'NONE', #5732, .T. ) ;
#17343 = VECTOR ( 'NONE', #15016, 999.9999999999998863 ) ;
#17344 = EDGE_CURVE ( 'NONE', #10794, #4259, #17939, .T. ) ;
#17345 = CARTESIAN_POINT ( 'NONE',  ( -13.20868407381886200, 370.9948905683720568, -6.410867750099233042 ) ) ;
#17346 = FACE_BOUND ( 'NONE', #14253, .T. ) ;
#17347 =( BOUNDED_CURVE ( )  B_SPLINE_CURVE ( 2, ( #2797, #4414, #5601, #4310, #7323, #17291, #10566, #20428, #8949, #15571, #7650, #4086, #757, #9058, #7212, #10997, #17401 ),
 .UNSPECIFIED., .F., .T. ) 
 B_SPLINE_CURVE_WITH_KNOTS ( ( 3, 2, 2, 2, 2, 2, 2, 2, 3 ),
 ( 0.6718750000000002220, 0.6738281250000002220, 0.6757812500000002220, 0.6777343750000002220, 0.6796875000000002220, 0.6816406250000002220, 0.6835937500000002220, 0.6855468750000002220, 0.6875000000000002220 ),
 .UNSPECIFIED. ) 
 CURVE ( )  GEOMETRIC_REPRESENTATION_ITEM ( )  RATIONAL_B_SPLINE_CURVE ( ( 0.9999999999999977796, 0.9807852804032326510, 1.000000000000000000, 0.9807852804032304306, 1.000000000000000000, 0.9807852804032304306, 1.000000000000000000, 0.9807852804032304306, 1.000000000000000000, 0.9807852804032304306, 1.000000000000000000, 0.9807852804032304306, 1.000000000000000000, 0.9807852804032304306, 1.000000000000000000, 0.9807852804032282101, 1.000000000000002220 ) ) 
 REPRESENTATION_ITEM ( '' )  );
#17348 = CARTESIAN_POINT ( 'NONE',  ( -36.33955658999053639, 509.1198905601784759, 18.47759065022572500 ) ) ;
#17349 = CARTESIAN_POINT ( 'NONE',  ( -32.01814843081344719, 346.0573905683720568, 16.75240474999999307 ) ) ;
#17350 = ORIENTED_EDGE ( 'NONE', *, *, #2631, .F. ) ;
#17351 = CARTESIAN_POINT ( 'NONE',  ( -35.09675569278796559, 511.9948905683720000, -15.47720386886985544 ) ) ;
#17352 = PRODUCT_DEFINITION_SHAPE ( 'NONE', 'NONE',  #21404 ) ;
#17353 = ORIENTED_EDGE ( 'NONE', *, *, #8898, .T. ) ;
#17354 = CARTESIAN_POINT ( 'NONE',  ( 60.03793209889851568, 30.52886280891152282, -131.1729372809869005 ) ) ;
#17355 = CARTESIAN_POINT ( 'NONE',  ( -35.09675569278795848, 417.2448905683720568, 15.47720386886985366 ) ) ;
#17356 = DIRECTION ( 'NONE',  ( 0.000000000000000000, -1.000000000000000000, 0.000000000000000000 ) ) ;
#17357 = DIRECTION ( 'NONE',  ( 0.000000000000000000, 0.000000000000000000, 1.000000000000000000 ) ) ;
#17358 = CARTESIAN_POINT ( 'NONE',  ( -13.20868407381887089, 468.2448905683720568, 6.410867750099229490 ) ) ;
#17359 = VECTOR ( 'NONE', #9728, 1000.000000000000000 ) ;
#17360 = EDGE_LOOP ( 'NONE', ( #14996, #19424, #11941, #5820 ) ) ;
#17361 = CARTESIAN_POINT ( 'NONE',  ( -11.93348319268873503, 468.5573905683720000, 3.332260488124728859 ) ) ;
#17362 = FACE_OUTER_BOUND ( 'NONE', #15371, .T. ) ;
#17363 = EDGE_CURVE ( 'NONE', #10360, #7385, #1300, .T. ) ;
#17364 = CARTESIAN_POINT ( 'NONE',  ( -14.54375231895777176, 395.7448905765656377, 14.14213562373094568 ) ) ;
#17365 = CARTESIAN_POINT ( 'NONE',  ( -10.20829729246297646, 277.6198905765655809, -7.653668647301794969 ) ) ;
#17366 = LINE ( 'NONE', #2653, #3366 ) ;
#17367 = CARTESIAN_POINT ( 'NONE',  ( 166.1493775951145437, 610.7448905601785327, 8.917803138848105604 ) ) ;
#17368 = CARTESIAN_POINT ( 'NONE',  ( -8.685887942688736985, 486.9948905765656377, -2.449293598294705724E-15 ) ) ;
#17369 = LINE ( 'NONE', #1356, #15793 ) ;
#17370 = CARTESIAN_POINT ( 'NONE',  ( -10.20829729246299422, 432.8698905601784759, -7.653668647301794969 ) ) ;
#17371 = CARTESIAN_POINT ( 'NONE',  ( 158.8141120573112630, 610.7448905601785327, 10.00000000000000888 ) ) ;
#17372 = AXIS2_PLACEMENT_3D ( 'NONE', #20507, #5571, #19093 ) ;
#17373 = CARTESIAN_POINT ( 'NONE',  ( -38.17536295476244845, 283.8073905683720568, -14.20200298773971426 ) ) ;
#17374 = EDGE_CURVE ( 'NONE', #19682, #15687, #11129, .T. ) ;
#17375 = CARTESIAN_POINT ( 'NONE',  ( -42.82802356641966668, 403.2448905765655809, 14.14213562373094923 ) ) ;
#17376 = CARTESIAN_POINT ( 'NONE',  ( -22.27502019258948351, 418.4948905683720000, 15.47720386886985189 ) ) ;
#17377 = CARTESIAN_POINT ( 'NONE',  ( 35.96497763894178945, 170.1716627696692683, -20.00000000000000355 ) ) ;
#17378 = CARTESIAN_POINT ( 'NONE',  ( -35.09675569278793716, 273.4948905683720000, -15.47720386886985544 ) ) ;
#17379 = VERTEX_POINT ( 'NONE', #16339 ) ;
#17380 = CARTESIAN_POINT ( 'NONE',  ( -14.54375231895778420, 478.2448905765655809, -14.14213562373094746 ) ) ;
#17381 = VERTEX_POINT ( 'NONE', #6468 ) ;
#17382 = CARTESIAN_POINT ( 'NONE',  ( -40.53162694259545162, 474.1198905683720568, -11.84573899990672707 ) ) ;
#17383 = EDGE_LOOP ( 'NONE', ( #18361, #15449, #1469, #16296 ) ) ;
#17384 = FACE_OUTER_BOUND ( 'NONE', #3282, .T. ) ;
#17385 = CARTESIAN_POINT ( 'NONE',  ( -28.68588794268870146, 241.3698905683720568, -16.75240474999999307 ) ) ;
#17386 = VECTOR ( 'NONE', #4649, 1000.000000000000000 ) ;
#17387 = EDGE_LOOP ( 'NONE', ( #20016, #3517, #10550, #12565, #3674, #8879 ) ) ;
#17388 = CARTESIAN_POINT ( 'NONE',  ( -45.43829269268873361, 524.1823905683721705, 3.332260488124734632 ) ) ;
#17389 = DIRECTION ( 'NONE',  ( -0.000000000000000000, 1.000000000000000000, -0.000000000000000000 ) ) ;
#17390 = ADVANCED_FACE ( 'NONE', ( #11237 ), #16123, .F. ) ;
#17391 = CARTESIAN_POINT ( 'NONE',  ( -45.64106924314020119, 472.9323905765655809, 11.32908994701042715 ) ) ;
#17392 = DIRECTION ( 'NONE',  ( 0.000000000000000000, 0.000000000000000000, 1.000000000000000000 ) ) ;
#17393 = LINE ( 'NONE', #6230, #21178 ) ;
#17394 = CARTESIAN_POINT ( 'NONE',  ( -36.09149475953510233, 223.9102039777116033, -15.70829946160876034 ) ) ;
#17395 = CARTESIAN_POINT ( 'NONE',  ( -48.68588794268873698, 573.2448905601785327, 0.000000000000000000 ) ) ;
#17396 = CARTESIAN_POINT ( 'NONE',  ( -14.48388495494901562, 509.4323905683719431, 9.489475012073732785 ) ) ;
#17397 = CARTESIAN_POINT ( 'NONE',  ( -3.905386575473828482E-15, 5.788408252967903067, 2.974182810908597041 ) ) ;
#17398 = CARTESIAN_POINT ( 'NONE',  ( -19.19641293061496867, 257.3073905683720568, 14.20200298773971426 ) ) ;
#17399 = CARTESIAN_POINT ( 'NONE',  ( -22.27502019258947286, 338.4948905683720568, 15.47720386886985189 ) ) ;
#17400 = VECTOR ( 'NONE', #14810, 1000.000000000000000 ) ;
#17401 = CARTESIAN_POINT ( 'NONE',  ( -48.68588794268870146, 317.2448905601784759, 0.000000000000000000 ) ) ;
#17402 = CARTESIAN_POINT ( 'NONE',  ( -36.33955658999050797, 273.8698905765656377, 18.47759065022572500 ) ) ;
#17403 = VECTOR ( 'NONE', #13917, 1000.000000000000000 ) ;
#17404 = CARTESIAN_POINT ( 'NONE',  ( -14.48388495494900496, 389.8073905683721136, -9.489475012073736337 ) ) ;
#17405 = CARTESIAN_POINT ( 'NONE',  ( -47.16347859291443712, 322.6198905765655809, 7.653668647301805628 ) ) ;
#17406 = CARTESIAN_POINT ( 'NONE',  ( -36.33955658999051508, 395.3698905601785327, -18.47759065022572855 ) ) ;
#17407 = EDGE_LOOP ( 'NONE', ( #20038, #20180, #19738, #7545, #8825, #17516 ) ) ;
#17408 = CARTESIAN_POINT ( 'NONE',  ( -28.68588794268874054, 573.2448905601785327, 0.000000000000000000 ) ) ;
#17409 = ORIENTED_EDGE ( 'NONE', *, *, #15379, .T. ) ;
#17410 = ORIENTED_EDGE ( 'NONE', *, *, #2578, .F. ) ;
#17411 = CARTESIAN_POINT ( 'NONE',  ( -11.93348319268873858, 500.0573905683720568, 3.332260488124728415 ) ) ;
#17412 = FACE_OUTER_BOUND ( 'NONE', #13642, .T. ) ;
#17413 = ORIENTED_EDGE ( 'NONE', *, *, #11556, .T. ) ;
#17414 = CARTESIAN_POINT ( 'NONE',  ( -14.48388495494899431, 311.3073905683720568, -9.489475012073734561 ) ) ;
#17415 = VERTEX_POINT ( 'NONE', #3133 ) ;
#17416 = CARTESIAN_POINT ( 'NONE',  ( -44.16309181155856578, 334.4948905683720568, 6.410867750099241924 ) ) ;
#17417 = CARTESIAN_POINT ( 'NONE',  ( -35.09675569278795138, 355.7448905683720568, 15.47720386886985366 ) ) ;
#17418 = AXIS2_PLACEMENT_3D ( 'NONE', #17839, #6369, #16344 ) ;
#17419 = CARTESIAN_POINT ( 'NONE',  ( -32.66413529028186957, 289.8073905765656946, -19.99999999999999289 ) ) ;
#17420 = CARTESIAN_POINT ( 'NONE',  ( -28.68588794268874054, 573.2448905601785327, 0.000000000000000000 ) ) ;
#17421 = CARTESIAN_POINT ( 'NONE',  ( -25.35362745456397704, 241.0573905683720000, -16.75240474999999307 ) ) ;
#17422 = CARTESIAN_POINT ( 'NONE',  ( -16.84014894278199392, 401.6198905683720568, -11.84573899990672707 ) ) ;
#17423 = CARTESIAN_POINT ( 'NONE',  ( -28.68588794268874054, 573.2448905601785327, 0.000000000000000000 ) ) ;
#17424 = CARTESIAN_POINT ( 'NONE',  ( -18.68588794268873698, 323.8848358243226357, 40.00000000000000000 ) ) ;
#17425 = DIRECTION ( 'NONE',  ( -1.000000000000000000, -1.374938938973709817E-16, 0.000000000000000000 ) ) ;
#17426 = EDGE_CURVE ( 'NONE', #15264, #8423, #11310, .T. ) ;
#17427 = CARTESIAN_POINT ( 'NONE',  ( -35.09675569278795848, 451.9948905683720000, -15.47720386886985544 ) ) ;
#17428 = ORIENTED_EDGE ( 'NONE', *, *, #9999, .F. ) ;
#17429 = CARTESIAN_POINT ( 'NONE',  ( -42.82802356641966668, 438.4948905601784759, 14.14213562373094923 ) ) ;
#17430 = ORIENTED_EDGE ( 'NONE', *, *, #14397, .F. ) ;
#17431 = ORIENTED_EDGE ( 'NONE', *, *, #15114, .T. ) ;
#17432 = VERTEX_POINT ( 'NONE', #4746 ) ;
#17433 = CARTESIAN_POINT ( 'NONE',  ( -28.68588794268872277, 250.8848358243226357, -40.00000000000000000 ) ) ;
#17434 = CARTESIAN_POINT ( 'NONE',  ( -11.73070664223724258, 331.3073905601785327, 11.32908994701042005 ) ) ;
#17435 = CARTESIAN_POINT ( 'NONE',  ( -28.68588794268871567, 372.8698905683720000, -16.75240474999999307 ) ) ;
#17436 = CARTESIAN_POINT ( 'NONE',  ( 91.21585410611801592, 31.85652257517428865, -40.00000000000000000 ) ) ;
#17437 = CARTESIAN_POINT ( 'NONE',  ( -40.01497788969916058, 520.4323905765656946, -16.95518130045146421 ) ) ;
#17438 = CARTESIAN_POINT ( 'NONE',  ( -14.48388495494900496, 407.9323905683720000, 9.489475012073732785 ) ) ;
#17439 = CARTESIAN_POINT ( 'NONE',  ( -14.48388495494898542, 241.3073905683720852, -9.489475012073736337 ) ) ;
#17440 = CARTESIAN_POINT ( 'NONE',  ( -14.48388495494900674, 397.9323905683720000, 9.489475012073731008 ) ) ;
#17441 = CARTESIAN_POINT ( 'NONE',  ( -8.685887942688719221, 337.3073905765655809, -3.978247347593165895 ) ) ;
#17442 = CARTESIAN_POINT ( 'NONE',  ( -13.20868407381885135, 298.2448905683720000, 6.410867750099229490 ) ) ;
#17443 = CARTESIAN_POINT ( 'NONE',  ( -38.17536295476246977, 453.8073905683720568, -14.20200298773971426 ) ) ;
#17444 = DIRECTION ( 'NONE',  ( -1.191790137725560488E-16, 1.000000000000000000, -0.000000000000000000 ) ) ;
#17445 = DIRECTION ( 'NONE',  ( 0.000000000000000000, -1.000000000000000000, 0.000000000000000000 ) ) ;
#17446 = CARTESIAN_POINT ( 'NONE',  ( 78.68120802659203150, 149.7457237375499517, 94.99999999999994316 ) ) ;
#17447 = CARTESIAN_POINT ( 'NONE',  ( -40.53162694259543741, 366.6198905683720000, 11.84573899990672885 ) ) ;
#17448 = CARTESIAN_POINT ( 'NONE',  ( -32.01814843081346140, 496.0573905683720568, 16.75240474999999307 ) ) ;
#17449 = CARTESIAN_POINT ( 'NONE',  ( -32.66413529028189799, 515.0573905601785327, -19.99999999999999289 ) ) ;
#17450 = CARTESIAN_POINT ( 'NONE',  ( -40.53162694259543741, 335.1198905683720568, 11.84573899990672885 ) ) ;
#17451 = ORIENTED_EDGE ( 'NONE', *, *, #15071, .F. ) ;
#17452 = CARTESIAN_POINT ( 'NONE',  ( -38.17536295476246266, 495.4323905683720000, 14.20200298773971781 ) ) ;
#17453 = ORIENTED_EDGE ( 'NONE', *, *, #17293, .T. ) ;
#17454 = FACE_BOUND ( 'NONE', #3754, .T. ) ;
#17455 = CARTESIAN_POINT ( 'NONE',  ( -25.35362745456399836, 432.5573905683719431, -16.75240474999999307 ) ) ;
#17456 = DIRECTION ( 'NONE',  ( 1.191790137725560488E-16, -1.000000000000000000, -0.000000000000000000 ) ) ;
#17457 = CARTESIAN_POINT ( 'NONE',  ( -10.20829729246300133, 492.8698905601784759, -7.653668647301794969 ) ) ;
#17458 = CARTESIAN_POINT ( 'NONE',  ( -45.43829269268871940, 474.1823905683720000, 3.332260488124734632 ) ) ;
#17459 = ORIENTED_EDGE ( 'NONE', *, *, #19055, .F. ) ;
#17460 = CARTESIAN_POINT ( 'NONE',  ( -11.93348319268873503, 468.8698905683720000, -2.051577885510841163E-15 ) ) ;
#17461 = CARTESIAN_POINT ( 'NONE',  ( -45.64106924314016567, 248.1823905601784759, 11.32908994701042538 ) ) ;
#17462 = CARTESIAN_POINT ( 'NONE',  ( -40.01497788969913927, 413.5573905765656946, 16.95518130045146776 ) ) ;
#17463 = PLANE ( 'NONE',  #333 ) ;
#17464 = CARTESIAN_POINT ( 'NONE',  ( -10.20829729246298712, 367.6198905765656377, -7.653668647301794969 ) ) ;
#17465 = CARTESIAN_POINT ( 'NONE',  ( -8.685887942688729879, 436.9948905765656377, -2.449293598294705724E-15 ) ) ;
#17466 = DIRECTION ( 'NONE',  ( -1.000000000000000000, -0.000000000000000000, -0.000000000000000000 ) ) ;
#17467 = FACE_BOUND ( 'NONE', #10745, .T. ) ;
#17468 = DIRECTION ( 'NONE',  ( -0.000000000000000000, -0.000000000000000000, 1.000000000000000000 ) ) ;
#17469 = EDGE_CURVE ( 'NONE', #8749, #17095, #499, .T. ) ;
#17470 = CARTESIAN_POINT ( 'NONE',  ( -48.68588794268854514, 346.9323905601784190, -3.978247347593583783 ) ) ;
#17471 =( BOUNDED_CURVE ( )  B_SPLINE_CURVE ( 2, ( #2286, #564, #7132, #3897, #15486, #672, #14405, #14187, #4330, #1102, #1204, #3998, #17525, #16023, #10913, #18816, #12443 ),
 .UNSPECIFIED., .F., .T. ) 
 B_SPLINE_CURVE_WITH_KNOTS ( ( 3, 2, 2, 2, 2, 2, 2, 2, 3 ),
 ( 0.6250000000000002220, 0.6269531250000002220, 0.6289062500000002220, 0.6308593750000002220, 0.6328125000000002220, 0.6347656250000002220, 0.6367187500000002220, 0.6386718750000002220, 0.6406250000000002220 ),
 .UNSPECIFIED. ) 
 CURVE ( )  GEOMETRIC_REPRESENTATION_ITEM ( )  RATIONAL_B_SPLINE_CURVE ( ( 0.9999999999999977796, 0.9807852804032326510, 1.000000000000000000, 0.9807852804032304306, 1.000000000000000000, 0.9807852804032304306, 1.000000000000000000, 0.9807852804032304306, 1.000000000000000000, 0.9807852804032304306, 1.000000000000000000, 0.9807852804032304306, 1.000000000000000000, 0.9807852804032304306, 1.000000000000000000, 0.9807852804032282101, 1.000000000000002220 ) ) 
 REPRESENTATION_ITEM ( '' )  );
#17472 = CARTESIAN_POINT ( 'NONE',  ( -11.73070664223723547, 243.1823905601784759, -11.32908994701042715 ) ) ;
#17473 = CARTESIAN_POINT ( 'NONE',  ( -47.16347859291444422, 362.6198905765656377, 7.653668647301805628 ) ) ;
#17474 = CARTESIAN_POINT ( 'NONE',  ( -28.68588794268872277, 432.8698905683720568, -16.75240474999999307 ) ) ;
#17475 = DIRECTION ( 'NONE',  ( 0.000000000000000000, -0.000000000000000000, -1.000000000000000000 ) ) ;
#17476 = CARTESIAN_POINT ( 'NONE',  ( -14.48388495494898542, 251.3073905683720284, -9.489475012073736337 ) ) ;
#17477 = ORIENTED_EDGE ( 'NONE', *, *, #14198, .T. ) ;
#17478 = EDGE_LOOP ( 'NONE', ( #8533, #9391, #2890, #16516 ) ) ;
#17479 = CARTESIAN_POINT ( 'NONE',  ( -8.685887942688735208, 476.9948905765656377, -2.449293598294705724E-15 ) ) ;
#17480 = VERTEX_POINT ( 'NONE', #8628 ) ;
#17481 = CARTESIAN_POINT ( 'NONE',  ( -42.88789093042844769, 486.3073905683720568, 9.489475012073734561 ) ) ;
#17482 = VERTEX_POINT ( 'NONE', #6794 ) ;
#17483 = DIRECTION ( 'NONE',  ( 1.000000000000000000, 0.000000000000000000, 0.000000000000000000 ) ) ;
#17484 = CARTESIAN_POINT ( 'NONE',  ( -45.43829269268869098, 243.5573905683720000, -3.332260488124726194 ) ) ;
#17485 = VERTEX_POINT ( 'NONE', #15363 ) ;
#17486 = CARTESIAN_POINT ( 'NONE',  ( -22.27502019258949773, 526.9948905683720568, 15.47720386886985189 ) ) ;
#17487 = CARTESIAN_POINT ( 'NONE',  ( 51.98438129372387806, 30.52886280891151216, -94.99999999999994316 ) ) ;
#17488 = EDGE_CURVE ( 'NONE', #984, #16828, #12093, .T. ) ;
#17489 = CIRCLE ( 'NONE', #18174, 125.0000000000000000 ) ;
#17490 = CARTESIAN_POINT ( 'NONE',  ( -21.03221929538693757, 468.8698905765656377, -18.47759065022572855 ) ) ;
#17491 = CARTESIAN_POINT ( 'NONE',  ( -36.33955658999051508, 349.1198905601784759, 18.47759065022572500 ) ) ;
#17492 = DIRECTION ( 'NONE',  ( 1.000000000000000000, 0.000000000000000000, 0.000000000000000000 ) ) ;
#17493 = CARTESIAN_POINT ( 'NONE',  ( -16.84014894278197616, 231.6198905683720000, -11.84573899990672707 ) ) ;
#17494 = AXIS2_PLACEMENT_3D ( 'NONE', #14697, #16317, #17916 ) ;
#17495 = CARTESIAN_POINT ( 'NONE',  ( -25.35362745456401257, 522.5573905683720568, -16.75240474999999307 ) ) ;
#17496 = CYLINDRICAL_SURFACE ( 'NONE', #12167, 49.60091809715359545 ) ;
#17497 = CARTESIAN_POINT ( 'NONE',  ( -16.84014894278196905, 227.6198905683720000, 11.84573899990672530 ) ) ;
#17498 = CARTESIAN_POINT ( 'NONE',  ( -32.01814843081344719, 347.5573905683720568, 16.75240474999999307 ) ) ;
#17499 = DIRECTION ( 'NONE',  ( 1.000000000000000000, 0.000000000000000000, -0.000000000000000000 ) ) ;
#17500 = CARTESIAN_POINT ( 'NONE',  ( -21.03221929538690205, 305.1198905765656377, 18.47759065022572500 ) ) ;
#17501 = EDGE_CURVE ( 'NONE', #11244, #8722, #2693, .T. ) ;
#17502 = VECTOR ( 'NONE', #17168, 1000.000000000000000 ) ;
#17503 = CARTESIAN_POINT ( 'NONE',  ( -25.35362745456398414, 376.6823905683720000, 16.75240474999998952 ) ) ;
#17504 = CARTESIAN_POINT ( 'NONE',  ( -21.03221929538690560, 325.1198905765655809, 18.47759065022572500 ) ) ;
#17505 = CARTESIAN_POINT ( 'NONE',  ( -11.73070664223725146, 391.3073905601784759, 11.32908994701042005 ) ) ;
#17506 = AXIS2_PLACEMENT_3D ( 'NONE', #6743, #1463, #19842 ) ;
#17507 = VERTEX_POINT ( 'NONE', #116 ) ;
#17508 = CARTESIAN_POINT ( 'NONE',  ( -14.54375231895777532, 403.4948905601784759, -14.14213562373094746 ) ) ;
#17509 = ORIENTED_EDGE ( 'NONE', *, *, #115, .F. ) ;
#17510 = ORIENTED_EDGE ( 'NONE', *, *, #14041, .F. ) ;
#17511 = CARTESIAN_POINT ( 'NONE',  ( -28.68588794268872988, 507.8698905683720568, 16.75240474999999307 ) ) ;
#17512 = CARTESIAN_POINT ( 'NONE',  ( 51.50493485826542184, 160.1716627696692683, 40.00000000000000000 ) ) ;
#17513 = ORIENTED_EDGE ( 'NONE', *, *, #9276, .F. ) ;
#17514 = EDGE_CURVE ( 'NONE', #6352, #13150, #6467, .T. ) ;
#17515 = CARTESIAN_POINT ( 'NONE',  ( -45.43829269268870519, 295.6823905683720000, 3.332260488124734632 ) ) ;
#17516 = ORIENTED_EDGE ( 'NONE', *, *, #17122, .F. ) ;
#17517 = CARTESIAN_POINT ( 'NONE',  ( -19.19641293061498288, 330.4323905683720000, -14.20200298773971603 ) ) ;
#17518 = CARTESIAN_POINT ( 'NONE',  ( -32.01814843081344719, 351.6823905683720000, -16.75240474999999307 ) ) ;
#17519 = VECTOR ( 'NONE', #6764, 1000.000000000000000 ) ;
#17520 = CARTESIAN_POINT ( 'NONE',  ( -45.64106924314017277, 262.9323905765656377, 11.32908994701042715 ) ) ;
#17521 = CARTESIAN_POINT ( 'NONE',  ( 5.074999999999999289, 6.500000000000000888, 0.000000000000000000 ) ) ;
#17522 = CARTESIAN_POINT ( 'NONE',  ( -45.43829269268869808, 243.8698905683720568, 0.000000000000000000 ) ) ;
#17523 = CARTESIAN_POINT ( 'NONE',  ( -38.17536295476246266, 403.8073905683721136, -14.20200298773971426 ) ) ;
#17524 = VECTOR ( 'NONE', #142, 1000.000000000000000 ) ;
#17525 = CARTESIAN_POINT ( 'NONE',  ( -14.54375231895776643, 333.4948905601784759, -14.14213562373094746 ) ) ;
#17526 = PLANE ( 'NONE',  #20413 ) ;
#17527 = DIRECTION ( 'NONE',  ( 1.000000000000000000, 0.000000000000000000, 0.000000000000000000 ) ) ;
#17528 = CARTESIAN_POINT ( 'NONE',  ( -13.20868407381886911, 448.2448905683720000, 6.410867750099229490 ) ) ;
#17529 = ORIENTED_EDGE ( 'NONE', *, *, #12715, .F. ) ;
#17530 = CARTESIAN_POINT ( 'NONE',  ( -11.73070664223726034, 443.1823905601784759, -11.32908994701042715 ) ) ;
#17531 = AXIS2_PLACEMENT_3D ( 'NONE', #16020, #7772, #14400 ) ;
#17532 = ORIENTED_EDGE ( 'NONE', *, *, #11425, .F. ) ;
#17533 = ORIENTED_EDGE ( 'NONE', *, *, #6426, .T. ) ;
#17534 = ORIENTED_EDGE ( 'NONE', *, *, #910, .F. ) ;
#17535 = DIRECTION ( 'NONE',  ( 0.000000000000000000, 0.000000000000000000, -1.000000000000000000 ) ) ;
#17536 = CARTESIAN_POINT ( 'NONE',  ( -24.70764059509555821, 334.4323905601784759, -19.99999999999999289 ) ) ;
#17537 = CIRCLE ( 'NONE', #18567, 175.0000000000000284 ) ;
#17538 = CARTESIAN_POINT ( 'NONE',  ( -35.09675569278795138, 367.2448905683720000, 15.47720386886985366 ) ) ;
#17539 = DIRECTION ( 'NONE',  ( -0.000000000000000000, 0.8660254037844382635, 0.5000000000000008882 ) ) ;
#17540 = CARTESIAN_POINT ( 'NONE',  ( -14.54375231895778775, 498.2448905765656377, -14.14213562373094746 ) ) ;
#17541 = CARTESIAN_POINT ( 'NONE',  ( -35.09675569278795138, 385.7448905683720000, 15.47720386886985366 ) ) ;
#17542 = CARTESIAN_POINT ( 'NONE',  ( -13.20868407381884602, 239.7448905683720000, 6.410867750099229490 ) ) ;
#17543 = EDGE_CURVE ( 'NONE', #6011, #19571, #14793, .T. ) ;
#17544 = CARTESIAN_POINT ( 'NONE',  ( -40.53162694259544452, 415.1198905683720000, 11.84573899990672885 ) ) ;
#17545 = EDGE_CURVE ( 'NONE', #9392, #15904, #13628, .T. ) ;
#17546 = CARTESIAN_POINT ( 'NONE',  ( -45.64106924314018698, 341.0573905765656946, -11.32908994701042715 ) ) ;
#17547 = DIRECTION ( 'NONE',  ( 0.000000000000000000, 1.000000000000000000, -0.000000000000000000 ) ) ;
#17548 = CARTESIAN_POINT ( 'NONE',  ( -35.09675569278793716, 301.9948905683720568, -15.47720386886985544 ) ) ;
#17549 = CARTESIAN_POINT ( 'NONE',  ( -16.84014894278200103, 451.6198905683720568, -11.84573899990672707 ) ) ;
#17550 = CYLINDRICAL_SURFACE ( 'NONE', #5424, 20.00000000000000000 ) ;
#17551 = DIRECTION ( 'NONE',  ( -0.000000000000000000, 1.000000000000000000, -0.000000000000000000 ) ) ;
#17552 = DIRECTION ( 'NONE',  ( 0.000000000000000000, 0.000000000000000000, -1.000000000000000000 ) ) ;
#17553 = EDGE_CURVE ( 'NONE', #18972, #4317, #13521, .T. ) ;
#17554 = CARTESIAN_POINT ( 'NONE',  ( -19.19641293061498644, 361.9323905683721136, -14.20200298773971603 ) ) ;
#17555 = CARTESIAN_POINT ( 'NONE',  ( -42.88789093042845479, 504.8073905683720568, 9.489475012073736337 ) ) ;
#17556 = CARTESIAN_POINT ( 'NONE',  ( -42.82802356641967378, 505.9948905601785327, -14.14213562373094746 ) ) ;
#17557 = CARTESIAN_POINT ( 'NONE',  ( -22.27502019258947286, 316.9948905683720568, 15.47720386886985189 ) ) ;
#17558 = EDGE_CURVE ( 'NONE', #20381, #9225, #17537, .T. ) ;
#17559 = VERTEX_POINT ( 'NONE', #8419 ) ;
#17560 = CARTESIAN_POINT ( 'NONE',  ( -44.16309181155857999, 494.4948905683720568, 6.410867750099241924 ) ) ;
#17561 = ORIENTED_EDGE ( 'NONE', *, *, #20302, .T. ) ;
#17562 = CYLINDRICAL_SURFACE ( 'NONE', #13967, 5.000000000000004441 ) ;
#17563 = AXIS2_PLACEMENT_3D ( 'NONE', #12938, #2884, #19419 ) ;
#17564 = CARTESIAN_POINT ( 'NONE',  ( -13.20868407381886733, 429.7448905683720000, 6.410867750099229490 ) ) ;
#17565 = DIRECTION ( 'NONE',  ( -1.191790137725560488E-16, 1.000000000000000000, -0.000000000000000000 ) ) ;
#17566 = CARTESIAN_POINT ( 'NONE',  ( -25.35362745456399125, 456.6823905683720000, 16.75240474999998952 ) ) ;
#17567 = ORIENTED_EDGE ( 'NONE', *, *, #18391, .T. ) ;
#17568 = CARTESIAN_POINT ( 'NONE',  ( -42.88789093042844769, 464.8073905683720000, 9.489475012073734561 ) ) ;
#17569 = CARTESIAN_POINT ( 'NONE',  ( -40.01497788969914637, 415.6823905601785327, -16.95518130045146421 ) ) ;
#17570 = ADVANCED_FACE ( 'NONE', ( #15251 ), #20215, .F. ) ;
#17571 = CARTESIAN_POINT ( 'NONE',  ( -14.54375231895777532, 398.2448905765655809, -14.14213562373094746 ) ) ;
#17572 = PLANE ( 'NONE',  #1029 ) ;
#17573 = DIRECTION ( 'NONE',  ( 0.000000000000000000, 0.000000000000000000, 1.000000000000000000 ) ) ;
#17574 = LINE ( 'NONE', #15648, #12572 ) ;
#17575 = DIRECTION ( 'NONE',  ( 1.000000000000000000, 0.000000000000000000, -0.000000000000000000 ) ) ;
#17576 = CARTESIAN_POINT ( 'NONE',  ( -8.685887942688729879, 426.9948905765656377, -2.449293598294705724E-15 ) ) ;
#17577 = CARTESIAN_POINT ( 'NONE',  ( -42.82802356641964536, 255.9948905601784759, -14.14213562373094746 ) ) ;
#17578 = CARTESIAN_POINT ( 'NONE',  ( -42.29072086064468294, 223.9102039777117170, 12.95568915141013200 ) ) ;
#17579 = AXIS2_PLACEMENT_3D ( 'NONE', #10964, #2442, #14348 ) ;
#17580 = CARTESIAN_POINT ( 'NONE',  ( -42.82802356641964536, 238.4948905601784759, 14.14213562373094923 ) ) ;
#17581 = CARTESIAN_POINT ( 'NONE',  ( -45.64106924314018698, 448.1823905601785327, 11.32908994701042538 ) ) ;
#17582 = CARTESIAN_POINT ( 'NONE',  ( -13.20868407381886733, 429.7448905683720000, 6.410867750099229490 ) ) ;
#17583 = CARTESIAN_POINT ( 'NONE',  ( -11.73070664223724968, 383.1823905601784190, -11.32908994701042538 ) ) ;
#17584 = CARTESIAN_POINT ( 'NONE',  ( -35.09675569278793716, 257.2448905683720000, 15.47720386886985366 ) ) ;
#17585 = VERTEX_POINT ( 'NONE', #543 ) ;
#17586 = CARTESIAN_POINT ( 'NONE',  ( -48.68588794268872277, 481.9948905765656377, 0.000000000000000000 ) ) ;
#17587 = ORIENTED_EDGE ( 'NONE', *, *, #7274, .T. ) ;
#17588 = CARTESIAN_POINT ( 'NONE',  ( -19.19641293061498999, 458.8073905683720000, 14.20200298773971426 ) ) ;
#17589 = CARTESIAN_POINT ( 'NONE',  ( -32.66413529028186247, 234.1823905765656662, 19.99999999999999289 ) ) ;
#17590 = VERTEX_POINT ( 'NONE', #18684 ) ;
#17591 = CARTESIAN_POINT ( 'NONE',  ( -36.33955658999050797, 365.3698905601784759, -18.47759065022572855 ) ) ;
#17592 = CARTESIAN_POINT ( 'NONE',  ( -11.93348319268870839, 249.1823905683720568, -3.332260488124732856 ) ) ;
#17593 = ORIENTED_EDGE ( 'NONE', *, *, #4848, .F. ) ;
#17594 = CARTESIAN_POINT ( 'NONE',  ( -32.01814843081346140, 516.0573905683720568, 16.75240474999999307 ) ) ;
#17595 = CARTESIAN_POINT ( 'NONE',  ( 154.7587007620219026, 620.7448905601785327, 10.81142786866622885 ) ) ;
#17596 = CIRCLE ( 'NONE', #11018, 10.00000000000000888 ) ;
#17597 = CARTESIAN_POINT ( 'NONE',  ( -40.01497788969914637, 463.5573905765656377, 16.95518130045146776 ) ) ;
#17598 = CARTESIAN_POINT ( 'NONE',  ( -28.68588794268875475, 600.7448905601785327, 0.000000000000000000 ) ) ;
#17599 = CARTESIAN_POINT ( 'NONE',  ( -11.73070664223723725, 286.0573905765655809, 11.32908994701042005 ) ) ;
#17600 = CARTESIAN_POINT ( 'NONE',  ( -37.18636649280855977, 223.9102039777115465, -14.87251219269597335 ) ) ;
#17601 = CARTESIAN_POINT ( 'NONE',  ( -42.88789093042841927, 224.4323905683720000, -9.489475012073734561 ) ) ;
#17602 =( BOUNDED_CURVE ( )  B_SPLINE_CURVE ( 2, ( #18870, #943, #19096, #7185, #726, #5465, #7296, #838, #4059, #13920, #5679, #12388, #10864, #18982, #10756, #7510, #2553 ),
 .UNSPECIFIED., .F., .T. ) 
 B_SPLINE_CURVE_WITH_KNOTS ( ( 3, 2, 2, 2, 2, 2, 2, 2, 3 ),
 ( 0.9218750000000001110, 0.9238281250000001110, 0.9257812500000001110, 0.9277343750000001110, 0.9296875000000001110, 0.9316406250000001110, 0.9335937500000001110, 0.9355468750000001110, 0.9375000000000001110 ),
 .UNSPECIFIED. ) 
 CURVE ( )  GEOMETRIC_REPRESENTATION_ITEM ( )  RATIONAL_B_SPLINE_CURVE ( ( 0.9999999999999988898, 0.9807852804032315408, 1.000000000000000000, 0.9807852804032304306, 1.000000000000000000, 0.9807852804032304306, 1.000000000000000000, 0.9807852804032304306, 1.000000000000000000, 0.9807852804032304306, 1.000000000000000000, 0.9807852804032304306, 1.000000000000000000, 0.9807852804032304306, 1.000000000000000000, 0.9807852804032293204, 1.000000000000001110 ) ) 
 REPRESENTATION_ITEM ( '' )  );
#17603 = CARTESIAN_POINT ( 'NONE',  ( -20.13121767714597610, 223.9102039777117739, 18.15005032320406642 ) ) ;
#17604 = CARTESIAN_POINT ( 'NONE',  ( -13.20868407381884602, 229.4948905683720284, -6.410867750099233042 ) ) ;
#17605 = CARTESIAN_POINT ( 'NONE',  ( -25.35362745456397704, 328.1823905683720568, 16.75240474999998952 ) ) ;
#17606 = CARTESIAN_POINT ( 'NONE',  ( -32.66413529028188378, 469.4323905601784759, 19.99999999999999289 ) ) ;
#17607 = CARTESIAN_POINT ( 'NONE',  ( 0.05613245601076813363, 1.278525034532179916, 6.500000000000000888 ) ) ;
#17608 = CARTESIAN_POINT ( 'NONE',  ( -45.43829269268869808, 305.0573905683720000, -3.332260488124726194 ) ) ;
#17609 = CIRCLE ( 'NONE', #16586, 125.0000000000000000 ) ;
#17610 = EDGE_CURVE ( 'NONE', #2934, #14145, #10140, .T. ) ;
#17611 = CARTESIAN_POINT ( 'NONE',  ( -19.19641293061498999, 380.4323905683720568, -14.20200298773971603 ) ) ;
#17612 = CARTESIAN_POINT ( 'NONE',  ( -16.84014894278201169, 521.6198905683719431, -11.84573899990672707 ) ) ;
#17613 = CARTESIAN_POINT ( 'NONE',  ( -17.35679799567830273, 393.8073905601785896, -16.95518130045146421 ) ) ;
#17614 = DIRECTION ( 'NONE',  ( 1.000000000000000000, 0.000000000000000000, 0.000000000000000000 ) ) ;
#17615 = ORIENTED_EDGE ( 'NONE', *, *, #18931, .F. ) ;
#17616 = ORIENTED_EDGE ( 'NONE', *, *, #20066, .F. ) ;
#17617 = CARTESIAN_POINT ( 'NONE',  ( -40.53162694259545162, 496.6198905683720000, 11.84573899990672885 ) ) ;
#17618 = PRODUCT_RELATED_PRODUCT_CATEGORY ( 'part', '', ( #9583 ) ) ;
#17619 = DIRECTION ( 'NONE',  ( -1.000000000000000000, 0.000000000000000000, 0.000000000000000000 ) ) ;
#17620 = ORIENTED_EDGE ( 'NONE', *, *, #17553, .T. ) ;
#17621 = CARTESIAN_POINT ( 'NONE',  ( -28.68588794268870501, 297.8698905683720000, 16.75240474999999307 ) ) ;
#17622 = CARTESIAN_POINT ( 'NONE',  ( -40.53162694259543031, 322.6198905683720568, -11.84573899990672707 ) ) ;
#17623 = EDGE_CURVE ( 'NONE', #368, #19523, #7671, .T. ) ;
#17624 = CARTESIAN_POINT ( 'NONE',  ( -8.685887942688712116, 266.9948905765656377, -2.449293598294705724E-15 ) ) ;
#17625 = FACE_OUTER_BOUND ( 'NONE', #19556, .T. ) ;
#17626 = CARTESIAN_POINT ( 'NONE',  ( -49.57497958038186425, 230.5765313837437418, -60.00000000000000000 ) ) ;
#17627 = CARTESIAN_POINT ( 'NONE',  ( -28.68588794268871922, 392.8698905683720000, -16.75240474999999307 ) ) ;
#17628 = DIRECTION ( 'NONE',  ( -1.191790137725560488E-16, 1.000000000000000000, -0.000000000000000000 ) ) ;
#17629 = VECTOR ( 'NONE', #12625, 1000.000000000000114 ) ;
#17630 = CARTESIAN_POINT ( 'NONE',  ( -28.68588794268869790, 213.9102039777116602, 0.000000000000000000 ) ) ;
#17631 = VECTOR ( 'NONE', #5559, 1000.000000000000000 ) ;
#17632 = CARTESIAN_POINT ( 'NONE',  ( -11.73070664223726745, 507.9323905765655809, -11.32908994701042538 ) ) ;
#17633 = EDGE_CURVE ( 'NONE', #13900, #18327, #17347, .T. ) ;
#17634 = CARTESIAN_POINT ( 'NONE',  ( -45.43829269268871229, 434.1823905683720568, 3.332260488124734632 ) ) ;
#17635 = VERTEX_POINT ( 'NONE', #12640 ) ;
#17636 = CARTESIAN_POINT ( 'NONE',  ( -11.73070664223725501, 441.3073905601784759, 11.32908994701042005 ) ) ;
#17637 = ORIENTED_EDGE ( 'NONE', *, *, #3797, .F. ) ;
#17638 = EDGE_LOOP ( 'NONE', ( #20875, #18881, #11891 ) ) ;
#17639 = ORIENTED_EDGE ( 'NONE', *, *, #15892, .T. ) ;
#17640 = DIRECTION ( 'NONE',  ( -0.000000000000000000, -0.000000000000000000, 1.000000000000000000 ) ) ;
#17641 = CARTESIAN_POINT ( 'NONE',  ( -17.35679799567829562, 323.8073905601784190, -16.95518130045146421 ) ) ;
#17642 = CARTESIAN_POINT ( 'NONE',  ( -45.42716650061694139, 223.9102039777116886, -0.8991096741133857151 ) ) ;
#17643 = CARTESIAN_POINT ( 'NONE',  ( -45.43829269268871229, 355.3698905683720568, 0.000000000000000000 ) ) ;
#17644 = VECTOR ( 'NONE', #19868, 1000.000000000000000 ) ;
#17645 = PLANE ( 'NONE',  #7280 ) ;
#17646 = AXIS2_PLACEMENT_3D ( 'NONE', #16024, #21089, #14506 ) ;
#17647 = CARTESIAN_POINT ( 'NONE',  ( -17.35679799567830983, 505.4323905765656377, 16.95518130045146421 ) ) ;
#17648 = CARTESIAN_POINT ( 'NONE',  ( -19.19641293061498999, 380.4323905683720568, -14.20200298773971603 ) ) ;
#17649 = CARTESIAN_POINT ( 'NONE',  ( 60.03793209889851568, 10.52886280891152104, -131.1729372809869005 ) ) ;
#17650 = CARTESIAN_POINT ( 'NONE',  ( -19.19641293061498288, 397.3073905683720000, 14.20200298773971426 ) ) ;
#17651 = CARTESIAN_POINT ( 'NONE',  ( -21.03221929538691981, 328.8698905765656377, -18.47759065022572855 ) ) ;
#17652 = LINE ( 'NONE', #7372, #6525 ) ;
#17653 = CARTESIAN_POINT ( 'NONE',  ( -42.88789093042842637, 304.8073905683720000, 9.489475012073734561 ) ) ;
#17654 = CARTESIAN_POINT ( 'NONE',  ( -22.27502019258948707, 448.4948905683720568, 15.47720386886985189 ) ) ;
#17656 = CARTESIAN_POINT ( 'NONE',  ( 30.42502041961814996, 180.1716627696692967, 20.00000000000000355 ) ) ;
#17655 = PRODUCT_DEFINITION_FORMATION_WITH_SPECIFIED_SOURCE ( 'ANY', '', #5946, .NOT_KNOWN. ) ;
#17657 = CARTESIAN_POINT ( 'NONE',  ( -21.03221929538690915, 370.3698905601784759, 18.47759065022572500 ) ) ;
#17658 = DIRECTION ( 'NONE',  ( 1.000000000000000000, 0.000000000000000000, -0.000000000000000000 ) ) ;
#17659 = AXIS2_PLACEMENT_3D ( 'NONE', #10541, #15435, #2342 ) ;
#17660 = CARTESIAN_POINT ( 'NONE',  ( -11.93348319268872260, 370.6823905683719431, -3.332260488124732856 ) ) ;
#17661 = CARTESIAN_POINT ( 'NONE',  ( -19.19641293061499709, 507.3073905683720568, 14.20200298773971426 ) ) ;
#17662 = CARTESIAN_POINT ( 'NONE',  ( -48.68588794268872277, 497.2448905601785327, 0.000000000000000000 ) ) ;
#17663 = CARTESIAN_POINT ( 'NONE',  ( -38.17536295476244845, 322.3073905683720568, -14.20200298773971426 ) ) ;
#17664 = ORIENTED_EDGE ( 'NONE', *, *, #20859, .T. ) ;
#17665 = CARTESIAN_POINT ( 'NONE',  ( -4.707244432207906043E-15, 5.469921996229797578, -3.525817189091414949 ) ) ;
#17666 = ORIENTED_EDGE ( 'NONE', *, *, #777, .F. ) ;
#17667 = PLANE ( 'NONE',  #15001 ) ;
#17668 = CARTESIAN_POINT ( 'NONE',  ( -42.88789093042844058, 416.3073905683720568, 9.489475012073734561 ) ) ;
#17669 = FILL_AREA_STYLE ('',( #17776 ) ) ;
#17670 = CARTESIAN_POINT ( 'NONE',  ( -16.84014894278199748, 437.6198905683720000, 11.84573899990672530 ) ) ;
#17671 = ORIENTED_EDGE ( 'NONE', *, *, #5335, .T. ) ;
#17672 = CARTESIAN_POINT ( 'NONE',  ( -44.16309181155858710, 463.2448905683720568, -6.410867750099231266 ) ) ;
#17673 = DIRECTION ( 'NONE',  ( 0.000000000000000000, -0.000000000000000000, 1.000000000000000000 ) ) ;
#17674 = EDGE_CURVE ( 'NONE', #17091, #14922, #17190, .T. ) ;
#17675 = CARTESIAN_POINT ( 'NONE',  ( -45.64106924314019409, 391.0573905765655809, -11.32908994701042715 ) ) ;
#17676 = LINE ( 'NONE', #10749, #20343 ) ;
#17677 = CIRCLE ( 'NONE', #20442, 10.00000000000000888 ) ;
#17678 = FACE_BOUND ( 'NONE', #15949, .T. ) ;
#17679 = DIRECTION ( 'NONE',  ( 0.000000000000000000, 0.9253149302858357794, -0.3791995250394160633 ) ) ;
#17680 = LINE ( 'NONE', #15965, #13923 ) ;
#17681 = EDGE_CURVE ( 'NONE', #3667, #14150, #11625, .T. ) ;
#17682 = ADVANCED_FACE ( 'NONE', ( #5923 ), #13951, .F. ) ;
#17683 = EDGE_CURVE ( 'NONE', #18164, #20120, #6420, .T. ) ;
#17684 = FACE_OUTER_BOUND ( 'NONE', #3198, .T. ) ;
#17685 = LINE ( 'NONE', #10094, #11431 ) ;
#17686 = CARTESIAN_POINT ( 'NONE',  ( -42.54924018682451958, 223.9102039777117454, 12.58112014037532411 ) ) ;
#17687 = CARTESIAN_POINT ( 'NONE',  ( -25.35362745456399836, 422.5573905683721136, -16.75240474999999307 ) ) ;
#17688 = CARTESIAN_POINT ( 'NONE',  ( -8.685887942688724550, 382.2448905601784759, -2.449293598294705724E-15 ) ) ;
#17689 = CARTESIAN_POINT ( 'NONE',  ( -32.01814843081343298, 243.1823905683720568, -16.75240474999999307 ) ) ;
#17690 = EDGE_CURVE ( 'NONE', #19655, #9392, #7812, .T. ) ;
#17691 = ORIENTED_EDGE ( 'NONE', *, *, #8363, .F. ) ;
#17692 = CARTESIAN_POINT ( 'NONE',  ( 60.69669829156632090, 56.85652257517428865, -94.99999999999994316 ) ) ;
#17693 = ORIENTED_EDGE ( 'NONE', *, *, #4299, .T. ) ;
#17694 = CARTESIAN_POINT ( 'NONE',  ( -13.20868407381887089, 459.7448905683720568, 6.410867750099229490 ) ) ;
#17695 = CARTESIAN_POINT ( 'NONE',  ( -32.66413529028186247, 229.8073905765656377, -19.99999999999999289 ) ) ;
#17696 = ORIENTED_EDGE ( 'NONE', *, *, #6229, .F. ) ;
#17697 = DIRECTION ( 'NONE',  ( 0.9864615503757148129, 0.000000000000000000, -0.1639927121256942455 ) ) ;
#17698 = CARTESIAN_POINT ( 'NONE',  ( -45.43829269268869098, 223.5573905683720284, -3.332260488124726194 ) ) ;
#17699 = EDGE_LOOP ( 'NONE', ( #20433, #17587, #10255, #17778 ) ) ;
#17700 = CARTESIAN_POINT ( 'NONE',  ( -38.17536295476246977, 525.4323905683720568, 14.20200298773971781 ) ) ;
#17701 = CARTESIAN_POINT ( 'NONE',  ( -71.26501780185373036, 213.9102039777116602, -25.00000000000000355 ) ) ;
#17702 = CARTESIAN_POINT ( 'NONE',  ( -24.70764059509556176, 454.8073905765655809, 19.99999999999998934 ) ) ;
#17703 = DIRECTION ( 'NONE',  ( 1.191790137725560488E-16, -1.000000000000000000, -0.000000000000000000 ) ) ;
#17704 = CARTESIAN_POINT ( 'NONE',  ( 292.4526463419396691, 308.2087638784415162, -40.00000000000000000 ) ) ;
#17705 = CARTESIAN_POINT ( 'NONE',  ( -45.64106924314016567, 241.0573905765656093, -11.32908994701042538 ) ) ;
#17706 = CARTESIAN_POINT ( 'NONE',  ( -21.03221929538690205, 290.3698905601784759, 18.47759065022572500 ) ) ;
#17707 = VECTOR ( 'NONE', #8274, 1000.000000000000000 ) ;
#17708 = CARTESIAN_POINT ( 'NONE',  ( -18.68939845611674144, 223.9102039777117170, 17.39761213591845390 ) ) ;
#17709 = CARTESIAN_POINT ( 'NONE',  ( -44.16309181155855867, 223.2448905683720568, -6.410867750099231266 ) ) ;
#17710 = CARTESIAN_POINT ( 'NONE',  ( -16.84014894278198327, 311.6198905683720000, -11.84573899990672707 ) ) ;
#17711 = CARTESIAN_POINT ( 'NONE',  ( -47.16347859291445133, 446.6198905601784759, -7.653668647301793193 ) ) ;
#17712 = CARTESIAN_POINT ( 'NONE',  ( -42.82802356641965957, 378.4948905601784759, 14.14213562373094923 ) ) ;
#17713 = CARTESIAN_POINT ( 'NONE',  ( -11.93348319268871727, 310.0573905683720568, 3.332260488124728415 ) ) ;
#17714 = CARTESIAN_POINT ( 'NONE',  ( -13.20868407381886023, 378.2448905683720000, 6.410867750099229490 ) ) ;
#17715 = CARTESIAN_POINT ( 'NONE',  ( -11.93348319268874214, 530.6823905683720568, -3.332260488124732856 ) ) ;
#17716 = VECTOR ( 'NONE', #11101, 1000.000000000000000 ) ;
#17717 = CARTESIAN_POINT ( 'NONE',  ( -10.20829729246298534, 361.6198905601784759, 7.653668647301790529 ) ) ;
#17718 = CARTESIAN_POINT ( 'NONE',  ( -8.685887942688594876, 402.5573905601784190, -3.978247347592846594 ) ) ;
#17719 = VERTEX_POINT ( 'NONE', #3977 ) ;
#17720 = CARTESIAN_POINT ( 'NONE',  ( -38.17536295476246977, 483.8073905683720000, -14.20200298773971426 ) ) ;
#17721 =( NAMED_UNIT ( * ) PLANE_ANGLE_UNIT ( ) SI_UNIT ( $, .RADIAN. ) );
#17722 = CARTESIAN_POINT ( 'NONE',  ( -14.48388495494899075, 297.9323905683720000, 9.489475012073732785 ) ) ;
#17723 = ADVANCED_BREP_SHAPE_REPRESENTATION ( '', ( #4225, #12794 ), #16261 ) ;
#17724 = VERTEX_POINT ( 'NONE', #20539 ) ;
#17725 =( BOUNDED_CURVE ( )  B_SPLINE_CURVE ( 2, ( #6385, #16359, #8003, #3160, #2948, #3374, #1326, #9527, #19692, #21321, #12787, #19380, #16252, #4667, #19486, #16146, #11584 ),
 .UNSPECIFIED., .F., .T. ) 
 B_SPLINE_CURVE_WITH_KNOTS ( ( 3, 2, 2, 2, 2, 2, 2, 2, 3 ),
 ( 0.3437500000000001110, 0.3457031250000001110, 0.3476562500000001110, 0.3496093750000001110, 0.3515625000000001110, 0.3535156250000001110, 0.3554687500000001110, 0.3574218750000001110, 0.3593750000000001110 ),
 .UNSPECIFIED. ) 
 CURVE ( )  GEOMETRIC_REPRESENTATION_ITEM ( )  RATIONAL_B_SPLINE_CURVE ( ( 0.9999999999999988898, 0.9807852804032315408, 1.000000000000000000, 0.9807852804032304306, 1.000000000000000000, 0.9807852804032304306, 1.000000000000000000, 0.9807852804032304306, 1.000000000000000000, 0.9807852804032304306, 1.000000000000000000, 0.9807852804032304306, 1.000000000000000000, 0.9807852804032304306, 1.000000000000000000, 0.9807852804032293204, 1.000000000000001110 ) ) 
 REPRESENTATION_ITEM ( '' )  );
#17726 = CARTESIAN_POINT ( 'NONE',  ( -40.53162694259543031, 284.1198905683720000, -11.84573899990672707 ) ) ;
#17727 = CARTESIAN_POINT ( 'NONE',  ( -11.93348319268871549, 318.8698905683720000, -2.051577885510841163E-15 ) ) ;
#17728 = EDGE_CURVE ( 'NONE', #8877, #952, #12311, .T. ) ;
#17729 = CARTESIAN_POINT ( 'NONE',  ( -42.82802356641964536, 263.2448905765656377, 14.14213562373094923 ) ) ;
#17730 = CARTESIAN_POINT ( 'NONE',  ( -48.68588794268858777, 476.9323905601784759, -3.978247347593477201 ) ) ;
#17731 = CARTESIAN_POINT ( 'NONE',  ( -25.35362745456397704, 231.0573905683720568, -16.75240474999999307 ) ) ;
#17732 = AXIS2_PLACEMENT_3D ( 'NONE', #17156, #16946, #13698 ) ;
#17733 = CARTESIAN_POINT ( 'NONE',  ( -45.43829269268871229, 375.3698905683720568, 0.000000000000000000 ) ) ;
#17734 = DIRECTION ( 'NONE',  ( 0.000000000000000000, -1.000000000000000000, 0.000000000000000000 ) ) ;
#17735 = CARTESIAN_POINT ( 'NONE',  ( -18.68588794268873698, 281.1055109169419666, 20.00000000000000355 ) ) ;
#17736 = EDGE_CURVE ( 'NONE', #21185, #15843, #12318, .T. ) ;
#17737 = CARTESIAN_POINT ( 'NONE',  ( -48.68588794268869435, 251.9948905765656093, 0.000000000000000000 ) ) ;
#17738 = CARTESIAN_POINT ( 'NONE',  ( -11.93348319268872970, 438.8698905683720568, -2.051577885510841163E-15 ) ) ;
#17739 = CARTESIAN_POINT ( 'NONE',  ( -18.81370552131603091, 600.7448905601785327, 6.112943483001358480 ) ) ;
#17740 = ORIENTED_EDGE ( 'NONE', *, *, #11864, .T. ) ;
#17741 = CARTESIAN_POINT ( 'NONE',  ( -24.70764059509557242, 454.4323905601784759, -19.99999999999999289 ) ) ;
#17742 = AXIS2_PLACEMENT_3D ( 'NONE', #1238, #21022, #14442 ) ;
#17743 = ORIENTED_EDGE ( 'NONE', *, *, #2411, .F. ) ;
#17744 = EDGE_LOOP ( 'NONE', ( #14304, #8695, #602, #12326 ) ) ;
#17745 = ORIENTED_EDGE ( 'NONE', *, *, #6774, .T. ) ;
#17746 = CARTESIAN_POINT ( 'NONE',  ( 10.41669750159067220, 217.7548513357008630, -60.00000000000000000 ) ) ;
#17747 = CARTESIAN_POINT ( 'NONE',  ( -40.01497788969912506, 328.8073905601784759, 16.95518130045146776 ) ) ;
#17748 = CARTESIAN_POINT ( 'NONE',  ( 21.30000000000000071, 4.052968581778165278E-16, -3.309499999999999886 ) ) ;
#17749 = AXIS2_PLACEMENT_3D ( 'NONE', #6157, #21204, #14410 ) ;
#17750 = CARTESIAN_POINT ( 'NONE',  ( -28.68588794268871212, 367.8698905683720000, 16.75240474999999307 ) ) ;
#17751 = CARTESIAN_POINT ( 'NONE',  ( 116.0391604516428430, 192.9550247130592027, -40.00000000000000000 ) ) ;
#17752 = CARTESIAN_POINT ( 'NONE',  ( -36.33955658999052929, 493.8698905765655809, 18.47759065022572500 ) ) ;
#17753 = CARTESIAN_POINT ( 'NONE',  ( -44.16309181155857289, 383.2448905683720000, -6.410867750099231266 ) ) ;
#17754 = CARTESIAN_POINT ( 'NONE',  ( -44.16309181155855157, 225.9948905683720284, 6.410867750099241924 ) ) ;
#17755 = CARTESIAN_POINT ( 'NONE',  ( -45.43829269268871940, 393.5573905683720000, -3.332260488124726638 ) ) ;
#17756 = EDGE_CURVE ( 'NONE', #2858, #9302, #7429, .T. ) ;
#17757 = CARTESIAN_POINT ( 'NONE',  ( -42.82802356641965957, 333.2448905765656377, 14.14213562373094923 ) ) ;
#17758 = LINE ( 'NONE', #13108, #8939 ) ;
#17759 = CARTESIAN_POINT ( 'NONE',  ( -22.27502019258947641, 280.7448905683720568, -15.47720386886985544 ) ) ;
#17760 = CARTESIAN_POINT ( 'NONE',  ( -28.68588794268872277, 447.8698905683720000, 16.75240474999999307 ) ) ;
#17761 = CYLINDRICAL_SURFACE ( 'NONE', #15812, 19.99999999999999645 ) ;
#17762 = CARTESIAN_POINT ( 'NONE',  ( 147.4234352242185935, 610.7448905601785327, 1.893624729818134345 ) ) ;
#17763 = DIRECTION ( 'NONE',  ( -1.000000000000000000, -0.000000000000000000, 0.000000000000000000 ) ) ;
#17764 = AXIS2_PLACEMENT_3D ( 'NONE', #9306, #15823, #12246 ) ;
#17765 = CARTESIAN_POINT ( 'NONE',  ( -25.35362745456398059, 348.1823905683720000, 16.75240474999998952 ) ) ;
#17766 = CARTESIAN_POINT ( 'NONE',  ( -14.48388495494901562, 507.9323905683720568, 9.489475012073732785 ) ) ;
#17767 = CARTESIAN_POINT ( 'NONE',  ( -10.20829729246300310, 511.6198905601785327, 7.653668647301790529 ) ) ;
#17768 = CARTESIAN_POINT ( 'NONE',  ( -19.19641293061497933, 317.3073905683720000, 14.20200298773971426 ) ) ;
#17769 = EDGE_CURVE ( 'NONE', #7734, #9623, #8173, .T. ) ;
#17770 = ORIENTED_EDGE ( 'NONE', *, *, #21255, .F. ) ;
#17771 = CARTESIAN_POINT ( 'NONE',  ( -45.64106924314020119, 526.3073905601785327, -11.32908994701042538 ) ) ;
#17772 = ORIENTED_EDGE ( 'NONE', *, *, #13604, .F. ) ;
#17773 = LINE ( 'NONE', #9544, #1182 ) ;
#17774 = CARTESIAN_POINT ( 'NONE',  ( -16.84014894278199392, 429.1198905683720000, 11.84573899990672530 ) ) ;
#17775 = CARTESIAN_POINT ( 'NONE',  ( -8.685887942688708563, 236.9948905765656377, -2.449293598294705724E-15 ) ) ;
#17776 = FILL_AREA_STYLE_COLOUR ( '', #17995 ) ;
#17777 = CARTESIAN_POINT ( 'NONE',  ( -38.17536295476245556, 435.4323905683720568, 14.20200298773971781 ) ) ;
#17778 = ORIENTED_EDGE ( 'NONE', *, *, #7481, .F. ) ;
#17779 = CARTESIAN_POINT ( 'NONE',  ( -16.84014894278200458, 470.1198905683720568, -11.84573899990672707 ) ) ;
#17780 = DIRECTION ( 'NONE',  ( 0.000000000000000000, -1.000000000000000000, 0.000000000000000000 ) ) ;
#17781 = CARTESIAN_POINT ( 'NONE',  ( -28.68588794268872277, 414.7448905601784759, -19.99999999999999289 ) ) ;
#17782 = EDGE_CURVE ( 'NONE', #18587, #13633, #1278, .T. ) ;
#17783 = CARTESIAN_POINT ( 'NONE',  ( -48.68588794268871567, 391.6823905765655809, -3.978247347593158345 ) ) ;
#17784 = DIRECTION ( 'NONE',  ( -1.191790137725560488E-16, 1.000000000000000000, -0.000000000000000000 ) ) ;
#17785 = DIRECTION ( 'NONE',  ( 1.191790137725560488E-16, -1.000000000000000000, -0.000000000000000000 ) ) ;
#17786 = CARTESIAN_POINT ( 'NONE',  ( -47.16347859291445133, 431.3698905765655809, -7.653668647301793193 ) ) ;
#17787 = CARTESIAN_POINT ( 'NONE',  ( -48.68588794268869435, 251.9948905765656093, 0.000000000000000000 ) ) ;
#17788 = DIRECTION ( 'NONE',  ( -0.9365583756827543516, 0.000000000000000000, 0.3505116388060184329 ) ) ;
#17789 = CARTESIAN_POINT ( 'NONE',  ( -47.16347859291443001, 256.6198905601784759, -7.653668647301793193 ) ) ;
#17790 = CARTESIAN_POINT ( 'NONE',  ( -21.03221929538691981, 344.1198905601784759, -18.47759065022572855 ) ) ;
#17791 = CARTESIAN_POINT ( 'NONE',  ( -25.35362745456398770, 418.1823905683720568, 16.75240474999998952 ) ) ;
#17792 = CARTESIAN_POINT ( 'NONE',  ( -8.685887942688720997, 336.9948905765656377, -2.449293598294705724E-15 ) ) ;
#17793 = CARTESIAN_POINT ( 'NONE',  ( -14.48388495494898365, 249.4323905683720000, 9.489475012073732785 ) ) ;
#17794 = EDGE_LOOP ( 'NONE', ( #6537, #11783, #5629, #8151, #3314, #19025, #18112, #5507 ) ) ;
#17796 = ORIENTED_EDGE ( 'NONE', *, *, #1583, .T. ) ;
#17795 = VECTOR ( 'NONE', #18895, 1000.000000000000000 ) ;
#17797 = CARTESIAN_POINT ( 'NONE',  ( -8.685887942688729879, 426.9948905765656377, -2.449293598294705724E-15 ) ) ;
#17798 = EDGE_LOOP ( 'NONE', ( #19449, #11708, #1315, #18536 ) ) ;
#17799 = CARTESIAN_POINT ( 'NONE',  ( -45.43829269268872650, 465.3698905683720000, 0.000000000000000000 ) ) ;
#17800 = CARTESIAN_POINT ( 'NONE',  ( -45.64106924314017277, 221.0573905765656093, -11.32908994701042715 ) ) ;
#17801 = VERTEX_POINT ( 'NONE', #7753 ) ;
#17802 = CARTESIAN_POINT ( 'NONE',  ( -1.025382690249029949, 135.1716627696692683, 25.00000000000000000 ) ) ;
#17803 = CARTESIAN_POINT ( 'NONE',  ( -45.43829269268869098, 224.1823905683720284, 3.332260488124734632 ) ) ;
#17804 = ORIENTED_EDGE ( 'NONE', *, *, #12135, .F. ) ;
#17805 = CARTESIAN_POINT ( 'NONE',  ( -14.48388495494901917, 529.8073905683720568, -9.489475012073734561 ) ) ;
#17806 = CARTESIAN_POINT ( 'NONE',  ( -28.68588794268874054, 573.2448905601785327, 0.000000000000000000 ) ) ;
#17807 = CARTESIAN_POINT ( 'NONE',  ( -11.73070664223725679, 446.0573905765656377, 11.32908994701042005 ) ) ;
#17808 = DIRECTION ( 'NONE',  ( -0.000000000000000000, -1.000000000000000000, -0.000000000000000000 ) ) ;
#17809 = DIRECTION ( 'NONE',  ( -0.000000000000000000, -1.000000000000000000, -0.000000000000000000 ) ) ;
#17810 = CARTESIAN_POINT ( 'NONE',  ( -28.68588794268870146, 239.4948905765656377, -19.99999999999999289 ) ) ;
#17811 = ADVANCED_FACE ( 'NONE', ( #13062 ), #12742, .F. ) ;
#17812 = DIRECTION ( 'NONE',  ( 0.000000000000000000, 0.000000000000000000, 1.000000000000000000 ) ) ;
#17813 = ADVANCED_FACE ( 'NONE', ( #11541 ), #11321, .F. ) ;
#17814 = DIRECTION ( 'NONE',  ( 0.1238475123623134638, -0.9177839099959486102, 0.3772724323803887114 ) ) ;
#17815 = CARTESIAN_POINT ( 'NONE',  ( -45.43829269268869098, 233.5573905683720568, -3.332260488124726194 ) ) ;
#17816 = CARTESIAN_POINT ( 'NONE',  ( -35.09675569278794427, 327.2448905683720000, 15.47720386886985366 ) ) ;
#17817 = CARTESIAN_POINT ( 'NONE',  ( 0.5805565836007647862, -3.752776749732576356, -6.500000000000000000 ) ) ;
#17818 = CARTESIAN_POINT ( 'NONE',  ( -13.20868407381885135, 299.7448905683720568, 6.410867750099229490 ) ) ;
#17819 = CARTESIAN_POINT ( 'NONE',  ( -11.93348319268872260, 369.1823905683720000, -3.332260488124732856 ) ) ;
#17820 = CARTESIAN_POINT ( 'NONE',  ( -32.01814843081346140, 523.1823905683720568, -16.75240474999999307 ) ) ;
#17821 = CARTESIAN_POINT ( 'NONE',  ( -14.54375231895776643, 360.9948905601784759, 14.14213562373094568 ) ) ;
#17822 = CARTESIAN_POINT ( 'NONE',  ( -32.66413529028187668, 405.0573905601785327, -19.99999999999999289 ) ) ;
#17823 = VERTEX_POINT ( 'NONE', #17817 ) ;
#17824 = CARTESIAN_POINT ( 'NONE',  ( -22.27502019258949773, 482.2448905683720568, -15.47720386886985544 ) ) ;
#17825 = LINE ( 'NONE', #12964, #5584 ) ;
#17826 = CARTESIAN_POINT ( 'NONE',  ( -44.16309181155855867, 284.4948905683720000, 6.410867750099241924 ) ) ;
#17827 = ORIENTED_EDGE ( 'NONE', *, *, #13398, .F. ) ;
#17828 = CARTESIAN_POINT ( 'NONE',  ( -25.35362745456398414, 292.5573905683720568, -16.75240474999999307 ) ) ;
#17829 = CARTESIAN_POINT ( 'NONE',  ( -38.17536295476244135, 315.4323905683720000, 14.20200298773971781 ) ) ;
#17830 = CARTESIAN_POINT ( 'NONE',  ( -21.03221929538691271, 258.8698905765656377, -18.47759065022572855 ) ) ;
#17831 = LINE ( 'NONE', #4643, #11728 ) ;
#17832 = CARTESIAN_POINT ( 'NONE',  ( -35.09675569278793716, 235.7448905683720000, 15.47720386886985366 ) ) ;
#17833 = CARTESIAN_POINT ( 'NONE',  ( -24.70764059509554045, 224.4323905601785043, -19.99999999999999289 ) ) ;
#17834 = CARTESIAN_POINT ( 'NONE',  ( -45.43829269268870519, 385.0573905683720000, -3.332260488124726194 ) ) ;
#17835 = DIRECTION ( 'NONE',  ( -0.6352526299242171604, 0.000000000000000000, -0.7723044064191046942 ) ) ;
#17836 = CARTESIAN_POINT ( 'NONE',  ( 0.000000000000000000, 135.1716627696692683, 0.000000000000000000 ) ) ;
#17837 = LINE ( 'NONE', #16342, #12894 ) ;
#17838 = CARTESIAN_POINT ( 'NONE',  ( -14.48388495494900496, 417.9323905683720568, 9.489475012073732785 ) ) ;
#17839 = CARTESIAN_POINT ( 'NONE',  ( 44.98449999999999704, 0.000000000000000000, 0.000000000000000000 ) ) ;
#17840 = ORIENTED_EDGE ( 'NONE', *, *, #17163, .T. ) ;
#17841 = CARTESIAN_POINT ( 'NONE',  ( -45.64106924314019409, 418.1823905601784759, 11.32908994701042715 ) ) ;
#17842 = ORIENTED_EDGE ( 'NONE', *, *, #14580, .T. ) ;
#17843 = ORIENTED_EDGE ( 'NONE', *, *, #9944, .T. ) ;
#17844 = ORIENTED_EDGE ( 'NONE', *, *, #18391, .F. ) ;
#17845 = CARTESIAN_POINT ( 'NONE',  ( -43.52342829599624707, 209.6345393943126396, -2.222589281884806756 ) ) ;
#17846 = CARTESIAN_POINT ( 'NONE',  ( -42.82802356641965247, 315.9948905601784759, -14.14213562373094746 ) ) ;
#17847 = DIRECTION ( 'NONE',  ( -1.000000000000000000, 0.000000000000000000, 0.000000000000000000 ) ) ;
#17848 = CARTESIAN_POINT ( 'NONE',  ( -19.19641293061497933, 348.8073905683720000, 14.20200298773971426 ) ) ;
#17849 = VECTOR ( 'NONE', #20171, 1000.000000000000000 ) ;
#17850 = ADVANCED_FACE ( 'NONE', ( #14804, #14589 ), #21387, .F. ) ;
#17851 = CARTESIAN_POINT ( 'NONE',  ( -8.685887942688740537, 496.6823905765656377, 3.978247347593161010 ) ) ;
#17852 = CARTESIAN_POINT ( 'NONE',  ( -28.68588794268871567, 376.3698905683720568, 16.75240474999999307 ) ) ;
#17853 = CARTESIAN_POINT ( 'NONE',  ( -38.17536295476243424, 226.9323905683720000, 14.20200298773971781 ) ) ;
#17854 = CARTESIAN_POINT ( 'NONE',  ( -11.93348319268872437, 389.1823905683720568, -3.332260488124732856 ) ) ;
#17855 = VECTOR ( 'NONE', #17444, 1000.000000000000000 ) ;
#17856 = CARTESIAN_POINT ( 'NONE',  ( -14.54375231895776110, 315.7448905765656377, 14.14213562373094568 ) ) ;
#17857 = DIRECTION ( 'NONE',  ( 0.9365583756827543516, -0.000000000000000000, -0.3505116388060184329 ) ) ;
#17858 = CARTESIAN_POINT ( 'NONE',  ( -28.68588794268870146, 286.3698905683720568, 16.75240474999999307 ) ) ;
#17859 = CARTESIAN_POINT ( 'NONE',  ( -32.01814843081345430, 443.1823905683720568, -16.75240474999999307 ) ) ;
#17860 = DIRECTION ( 'NONE',  ( 0.000000000000000000, 0.000000000000000000, 1.000000000000000000 ) ) ;
#17861 = CARTESIAN_POINT ( 'NONE',  ( 0.000000000000000000, 5.629165124598848102, 3.250000000000005329 ) ) ;
#17862 = DIRECTION ( 'NONE',  ( -1.191790137725560488E-16, 1.000000000000000000, -0.000000000000000000 ) ) ;
#17863 = CIRCLE ( 'NONE', #15805, 10.00000000000000178 ) ;
#17864 = CARTESIAN_POINT ( 'NONE',  ( -38.17536295476244845, 356.9323905683720000, 14.20200298773971781 ) ) ;
#17865 = CARTESIAN_POINT ( 'NONE',  ( -28.68588794268873343, 501.3698905683721136, -16.75240474999999307 ) ) ;
#17866 = CARTESIAN_POINT ( 'NONE',  ( -10.20829729246299955, 481.6198905601785327, 7.653668647301790529 ) ) ;
#17867 = CARTESIAN_POINT ( 'NONE',  ( -45.43829269268870519, 333.5573905683720568, -3.332260488124726194 ) ) ;
#17868 = EDGE_CURVE ( 'NONE', #11758, #12542, #12956, .T. ) ;
#17869 = AXIS2_PLACEMENT_3D ( 'NONE', #11020, #17628, #9404 ) ;
#17870 = VERTEX_POINT ( 'NONE', #6344 ) ;
#17871 = CARTESIAN_POINT ( 'NONE',  ( 91.21585410611801592, 56.85652257517428865, 94.99999999999994316 ) ) ;
#17872 = PRODUCT_DEFINITION_SHAPE ( 'NONE', 'NONE',  #21397 ) ;
#17873 = EDGE_LOOP ( 'NONE', ( #2916, #3655, #7229, #17529, #18694 ) ) ;
#17874 = CARTESIAN_POINT ( 'NONE',  ( 60.74769842942832554, 56.85652257517428865, 40.00000000000000000 ) ) ;
#17875 = CARTESIAN_POINT ( 'NONE',  ( -11.93348319268872615, 410.0573905683720568, 3.332260488124728859 ) ) ;
#17876 = CYLINDRICAL_SURFACE ( 'NONE', #5895, 19.99999999999999645 ) ;
#17877 = CARTESIAN_POINT ( 'NONE',  ( -25.35362745456400191, 451.0573905683719431, -16.75240474999999307 ) ) ;
#17878 = CARTESIAN_POINT ( 'NONE',  ( -38.17536295476246266, 455.4323905683720568, 14.20200298773971781 ) ) ;
#17879 = DIRECTION ( 'NONE',  ( 0.000000000000000000, 0.000000000000000000, -1.000000000000000000 ) ) ;
#17880 = CYLINDRICAL_SURFACE ( 'NONE', #5184, 9.999999999999994671 ) ;
#17881 = CARTESIAN_POINT ( 'NONE',  ( -11.73070664223725323, 387.9323905765656377, -11.32908994701042715 ) ) ;
#17882 = CARTESIAN_POINT ( 'NONE',  ( -8.685887942688724550, 366.9948905765655809, -2.449293598294705724E-15 ) ) ;
#17883 = CARTESIAN_POINT ( 'NONE',  ( -45.64106924314018698, 391.0573905765656377, -11.32908994701042538 ) ) ;
#17884 = CARTESIAN_POINT ( 'NONE',  ( 88.28695088269886071, 142.5259582928263455, -40.00000000000000000 ) ) ;
#17885 = CARTESIAN_POINT ( 'NONE',  ( -47.16347859291443001, 252.6198905765656377, 7.653668647301805628 ) ) ;
#17886 = CARTESIAN_POINT ( 'NONE',  ( -22.27502019258949062, 488.4948905683720568, 15.47720386886985189 ) ) ;
#17887 = EDGE_CURVE ( 'NONE', #16993, #16325, #2697, .T. ) ;
#17888 = DIRECTION ( 'NONE',  ( 0.000000000000000000, 1.000000000000000000, 0.000000000000000000 ) ) ;
#17889 = DIRECTION ( 'NONE',  ( -0.000000000000000000, -0.000000000000000000, -1.000000000000000000 ) ) ;
#17890 = CARTESIAN_POINT ( 'NONE',  ( -28.68588794268871212, 344.7448905601784759, -19.99999999999999289 ) ) ;
#17891 = CARTESIAN_POINT ( 'NONE',  ( -13.20868407381886378, 409.7448905683720000, 6.410867750099229490 ) ) ;
#17892 = FACE_OUTER_BOUND ( 'NONE', #6646, .T. ) ;
#17893 = CARTESIAN_POINT ( 'NONE',  ( -28.68588794268870146, 252.8698905683720000, -16.75240474999999307 ) ) ;
#17894 = EDGE_CURVE ( 'NONE', #795, #12450, #11426, .T. ) ;
#17895 = ORIENTED_EDGE ( 'NONE', *, *, #5130, .T. ) ;
#17896 = FACE_OUTER_BOUND ( 'NONE', #12801, .T. ) ;
#17897 = EDGE_LOOP ( 'NONE', ( #12433, #15873, #17172, #18484 ) ) ;
#17898 = CARTESIAN_POINT ( 'NONE',  ( -16.84014894278200458, 471.6198905683720000, -11.84573899990672707 ) ) ;
#17899 = CARTESIAN_POINT ( 'NONE',  ( -10.20829729246297113, 226.3698905765656377, 7.653668647301790529 ) ) ;
#17900 = ORIENTED_EDGE ( 'NONE', *, *, #10318, .F. ) ;
#17901 = CARTESIAN_POINT ( 'NONE',  ( -42.82802356641968089, 523.2448905765656946, 14.14213562373094923 ) ) ;
#17902 = CARTESIAN_POINT ( 'NONE',  ( -42.88789093042845479, 534.4323905683720568, -9.489475012073736337 ) ) ;
#17903 = ORIENTED_EDGE ( 'NONE', *, *, #10809, .F. ) ;
#17904 = CARTESIAN_POINT ( 'NONE',  ( -28.68588794268873343, 501.3698905683721136, -16.75240474999999307 ) ) ;
#17905 = DIRECTION ( 'NONE',  ( 0.02112707654195870172, -0.9250389998264586522, -0.3792841882241536067 ) ) ;
#17906 = CARTESIAN_POINT ( 'NONE',  ( -48.68588794268871567, 441.6823905765656377, -3.978247347593158345 ) ) ;
#17907 = CARTESIAN_POINT ( 'NONE',  ( -36.33955658999050087, 300.1198905765656377, -18.47759065022572855 ) ) ;
#17908 = CARTESIAN_POINT ( 'NONE',  ( -22.27502019258947641, 346.9948905683720000, 15.47720386886985189 ) ) ;
#17909 = CARTESIAN_POINT ( 'NONE',  ( -8.685887942688886199, 456.6823905765655809, 3.978247347593533600 ) ) ;
#17910 = FACE_BOUND ( 'NONE', #15471, .T. ) ;
#17911 = LINE ( 'NONE', #1381, #8417 ) ;
#17912 = VECTOR ( 'NONE', #16413, 1000.000000000000000 ) ;
#17913 = CARTESIAN_POINT ( 'NONE',  ( -23.15340224802397273, 223.9102039777117739, 19.28725776582380647 ) ) ;
#17914 = CARTESIAN_POINT ( 'NONE',  ( -42.88789093042841927, 222.9323905683720284, -9.489475012073736337 ) ) ;
#17915 = CARTESIAN_POINT ( 'NONE',  ( -11.93348319268871549, 320.3698905683720568, -2.051577885510841163E-15 ) ) ;
#17916 = DIRECTION ( 'NONE',  ( -1.000000000000000000, 0.000000000000000000, -0.000000000000000000 ) ) ;
#17917 = CARTESIAN_POINT ( 'NONE',  ( -36.33955658999050797, 279.1198905601784759, 18.47759065022572500 ) ) ;
#17918 = DIRECTION ( 'NONE',  ( -0.000000000000000000, -1.000000000000000000, -0.000000000000000000 ) ) ;
#17919 = CARTESIAN_POINT ( 'NONE',  ( -28.68588794268870501, 307.8698905683720000, 16.75240474999999307 ) ) ;
#17920 = CARTESIAN_POINT ( 'NONE',  ( -42.88789093042845479, 514.4323905683720568, -9.489475012073734561 ) ) ;
#17921 = CARTESIAN_POINT ( 'NONE',  ( -32.66413529028187668, 375.0573905601784759, -19.99999999999999289 ) ) ;
#17922 = VECTOR ( 'NONE', #14212, 1000.000000000000000 ) ;
#17923 = CARTESIAN_POINT ( 'NONE',  ( -21.03221929538690915, 228.8698905765655809, -18.47759065022572855 ) ) ;
#17924 = ORIENTED_EDGE ( 'NONE', *, *, #3873, .F. ) ;
#17925 = CARTESIAN_POINT ( 'NONE',  ( -13.20868407381887266, 479.7448905683720568, 6.410867750099229490 ) ) ;
#17926 = CARTESIAN_POINT ( 'NONE',  ( -49.57497958038186425, 230.5765313837437418, -49.99999999999999289 ) ) ;
#17927 = CARTESIAN_POINT ( 'NONE',  ( -40.53162694259543031, 272.6198905683720568, -11.84573899990672707 ) ) ;
#17928 = VERTEX_POINT ( 'NONE', #18027 ) ;
#17929 = CARTESIAN_POINT ( 'NONE',  ( -16.84014894278197971, 281.6198905683720000, -11.84573899990672707 ) ) ;
#17930 = AXIS2_PLACEMENT_3D ( 'NONE', #1816, #16941, #15216 ) ;
#17931 = CARTESIAN_POINT ( 'NONE',  ( -14.48388495494899431, 319.8073905683720568, -9.489475012073736337 ) ) ;
#17932 = ADVANCED_FACE ( 'NONE', ( #9383 ), #11219, .F. ) ;
#17933 = CARTESIAN_POINT ( 'NONE',  ( -32.66413529028186247, 259.8073905765655809, -19.99999999999999289 ) ) ;
#17934 = CARTESIAN_POINT ( 'NONE',  ( 6.416697501590670427, 217.7548513357008630, -49.99999999999999289 ) ) ;
#17935 = CARTESIAN_POINT ( 'NONE',  ( -38.17536295476244135, 232.3073905683720568, -14.20200298773971426 ) ) ;
#17936 = EDGE_CURVE ( 'NONE', #20007, #8266, #8496, .T. ) ;
#17937 = CARTESIAN_POINT ( 'NONE',  ( -44.16309181155856578, 375.9948905683720568, 6.410867750099241924 ) ) ;
#17938 = EDGE_CURVE ( 'NONE', #8292, #6060, #8148, .T. ) ;
#17939 = LINE ( 'NONE', #21087, #20642 ) ;
#17940 = DIRECTION ( 'NONE',  ( -1.000000000000000000, -0.000000000000000000, 0.000000000000000000 ) ) ;
#17941 = CARTESIAN_POINT ( 'NONE',  ( -162.2727221670389781, 30.52886280891152282, 20.57735571454641033 ) ) ;
#17942 = CARTESIAN_POINT ( 'NONE',  ( -42.88789093042844058, 422.9323905683720000, -9.489475012073736337 ) ) ;
#17943 = PLANE ( 'NONE',  #19825 ) ;
#17944 = ORIENTED_EDGE ( 'NONE', *, *, #12663, .F. ) ;
#17945 = CARTESIAN_POINT ( 'NONE',  ( -21.03221929538693047, 434.1198905601784759, -18.47759065022572855 ) ) ;
#17946 = EDGE_CURVE ( 'NONE', #13870, #16962, #8714, .T. ) ;
#17947 = EDGE_LOOP ( 'NONE', ( #18828, #19286 ) ) ;
#17948 = ORIENTED_EDGE ( 'NONE', *, *, #7630, .T. ) ;
#17949 = ORIENTED_EDGE ( 'NONE', *, *, #4677, .F. ) ;
#17950 = PLANE ( 'NONE',  #10782 ) ;
#17951 = CARTESIAN_POINT ( 'NONE',  ( -45.64106924314017988, 298.1823905601784759, 11.32908994701042715 ) ) ;
#17952 = CARTESIAN_POINT ( 'NONE',  ( -28.68588794268874054, 588.2448905601785327, 0.000000000000000000 ) ) ;
#17953 = CARTESIAN_POINT ( 'NONE',  ( -32.01814843081344719, 353.1823905683720568, -16.75240474999999307 ) ) ;
#17954 = CARTESIAN_POINT ( 'NONE',  ( -17.35679799567830983, 495.4323905765656377, 16.95518130045146421 ) ) ;
#17955 = CARTESIAN_POINT ( 'NONE',  ( -32.01814843081344719, 381.6823905683719431, -16.75240474999999307 ) ) ;
#17956 = CARTESIAN_POINT ( 'NONE',  ( -71.26501780185373036, 135.1716627696692683, 25.00000000000000355 ) ) ;
#17957 = CARTESIAN_POINT ( 'NONE',  ( -28.68588794268871567, 376.3698905683720568, 16.75240474999999307 ) ) ;
#17958 = CARTESIAN_POINT ( 'NONE',  ( -36.33955658999050797, 330.1198905765655809, -18.47759065022572855 ) ) ;
#17959 = DIRECTION ( 'NONE',  ( 0.000000000000000000, 0.000000000000000000, 1.000000000000000000 ) ) ;
#17960 = CARTESIAN_POINT ( 'NONE',  ( -42.88789093042842637, 282.9323905683720568, -9.489475012073734561 ) ) ;
#17961 = CARTESIAN_POINT ( 'NONE',  ( -19.19641293061498999, 438.8073905683720000, 14.20200298773971426 ) ) ;
#17962 = CARTESIAN_POINT ( 'NONE',  ( 4.700000000000000178, 3.752776749732560368, -6.499999999999999112 ) ) ;
#17963 = FACE_OUTER_BOUND ( 'NONE', #11271, .T. ) ;
#17964 =( BOUNDED_CURVE ( )  B_SPLINE_CURVE ( 2, ( #8914, #3945, #10530, #5993, #15535, #12381, #9126, #19088, #716, #17257, #7288, #5671, #20711, #17461, #5884, #9236, #14763 ),
 .UNSPECIFIED., .F., .T. ) 
 B_SPLINE_CURVE_WITH_KNOTS ( ( 3, 2, 2, 2, 2, 2, 2, 2, 3 ),
 ( 0.8906250000000002220, 0.8925781250000002220, 0.8945312500000002220, 0.8964843750000002220, 0.8984375000000002220, 0.9003906250000001110, 0.9023437500000001110, 0.9042968750000001110, 0.9062500000000001110 ),
 .UNSPECIFIED. ) 
 CURVE ( )  GEOMETRIC_REPRESENTATION_ITEM ( )  RATIONAL_B_SPLINE_CURVE ( ( 0.9999999999999977796, 0.9807852804032326510, 1.000000000000000000, 0.9807852804032304306, 1.000000000000000000, 0.9807852804032304306, 1.000000000000000000, 0.9807852804032304306, 1.000000000000000000, 0.9807852804032304306, 1.000000000000000000, 0.9807852804032304306, 1.000000000000000000, 0.9807852804032304306, 1.000000000000000000, 0.9807852804032293204, 1.000000000000001110 ) ) 
 REPRESENTATION_ITEM ( '' )  );
#17965 = CARTESIAN_POINT ( 'NONE',  ( -40.01497788969913927, 448.8073905601785327, 16.95518130045146776 ) ) ;
#17966 = CARTESIAN_POINT ( 'NONE',  ( -16.84014894278198682, 341.6198905683720000, -11.84573899990672707 ) ) ;
#17967 = CARTESIAN_POINT ( 'NONE',  ( -40.53162694259545162, 482.6198905683720000, -11.84573899990672707 ) ) ;
#17968 = ORIENTED_EDGE ( 'NONE', *, *, #13066, .T. ) ;
#17969 = CARTESIAN_POINT ( 'NONE',  ( -36.33955658999052218, 495.3698905601784759, -18.47759065022572855 ) ) ;
#17970 = CARTESIAN_POINT ( 'NONE',  ( -11.93348319268871549, 308.8698905683720000, -2.051577885510841163E-15 ) ) ;
#17971 = ORIENTED_EDGE ( 'NONE', *, *, #4719, .T. ) ;
#17972 = VECTOR ( 'NONE', #16167, 1000.000000000000000 ) ;
#17973 = AXIS2_PLACEMENT_3D ( 'NONE', #227, #16550, #1736 ) ;
#17974 = CARTESIAN_POINT ( 'NONE',  ( 0.000000000000000000, 0.000000000000000000, 0.000000000000000000 ) ) ;
#17975 = ORIENTED_EDGE ( 'NONE', *, *, #17469, .F. ) ;
#17976 = DIRECTION ( 'NONE',  ( -1.000000000000000000, -0.000000000000000000, -0.000000000000000000 ) ) ;
#17978 = VECTOR ( 'NONE', #16040, 1000.000000000000000 ) ;
#17977 = APPLICATION_CONTEXT ( 'automotive_design' ) ;
#17979 = CARTESIAN_POINT ( 'NONE',  ( -28.68588794268872277, 412.8698905683720568, -16.75240474999999307 ) ) ;
#17980 = CARTESIAN_POINT ( 'NONE',  ( -17.35679799567827786, 235.4323905765656093, 16.95518130045146421 ) ) ;
#17981 =( NAMED_UNIT ( * ) PLANE_ANGLE_UNIT ( ) SI_UNIT ( $, .RADIAN. ) );
#17982 = CARTESIAN_POINT ( 'NONE',  ( -22.27502019258949773, 440.7448905683720000, -15.47720386886985544 ) ) ;
#17983 = AXIS2_PLACEMENT_3D ( 'NONE', #16196, #6335, #1375 ) ;
#17984 = CARTESIAN_POINT ( 'NONE',  ( -44.16309181155857999, 443.2448905683720000, -6.410867750099231266 ) ) ;
#17985 = DIRECTION ( 'NONE',  ( 0.7730552708769987680, -0.6343386699305746390, 0.000000000000000000 ) ) ;
#17986 = DIRECTION ( 'NONE',  ( -0.9864615503757148129, 0.000000000000000000, 0.1639927121256943010 ) ) ;
#17987 = PRODUCT_DEFINITION_FORMATION_WITH_SPECIFIED_SOURCE ( 'ANY', '', #19255, .NOT_KNOWN. ) ;
#17988 = CARTESIAN_POINT ( 'NONE',  ( -42.82802356641965957, 380.7448905765656377, -14.14213562373094746 ) ) ;
#17989 = CARTESIAN_POINT ( 'NONE',  ( -48.68588794268870856, 381.9948905765655809, 0.000000000000000000 ) ) ;
#17990 = FACE_OUTER_BOUND ( 'NONE', #13441, .T. ) ;
#17991 = CARTESIAN_POINT ( 'NONE',  ( -45.64106924314018698, 431.0573905765655809, -11.32908994701042538 ) ) ;
#17992 = CARTESIAN_POINT ( 'NONE',  ( -8.685887942688735208, 588.2448905601785327, 0.000000000000000000 ) ) ;
#17993 = CARTESIAN_POINT ( 'NONE',  ( -45.43829269268871940, 495.6823905683720568, 3.332260488124734632 ) ) ;
#17994 = EDGE_CURVE ( 'NONE', #17870, #4866, #4896, .T. ) ;
#17995 = COLOUR_RGB ( '',0.7921568627450980005, 0.8196078431372548767, 0.9333333333333333481 ) ;
#17996 = DIRECTION ( 'NONE',  ( -1.000000000000000000, 0.000000000000000000, -0.000000000000000000 ) ) ;
#17997 = CIRCLE ( 'NONE', #9369, 6.500000000000000888 ) ;
#17998 = CARTESIAN_POINT ( 'NONE',  ( -28.68588794268875475, 600.7448905601785327, 0.000000000000000000 ) ) ;
#17999 = CARTESIAN_POINT ( 'NONE',  ( -42.83990393396077678, 205.8064044967071879, 4.966739033517835189 ) ) ;
#18000 = CARTESIAN_POINT ( 'NONE',  ( -28.68588794268871922, 402.8698905683720000, -16.75240474999999307 ) ) ;
#18001 = CARTESIAN_POINT ( 'NONE',  ( -17.35679799567830983, 468.5573905765655240, -16.95518130045146421 ) ) ;
#18002 = EDGE_CURVE ( 'NONE', #9723, #10312, #16528, .T. ) ;
#18003 = CARTESIAN_POINT ( 'NONE',  ( -28.68588794268869435, 227.8698905683720284, 16.75240474999999307 ) ) ;
#18004 = ORIENTED_EDGE ( 'NONE', *, *, #16983, .F. ) ;
#18005 = FACE_OUTER_BOUND ( 'NONE', #3361, .T. ) ;
#18006 = VERTEX_POINT ( 'NONE', #1713 ) ;
#18007 = CARTESIAN_POINT ( 'NONE',  ( -19.19641293061499709, 471.9323905683720568, -14.20200298773971603 ) ) ;
#18008 = CARTESIAN_POINT ( 'NONE',  ( -47.16347859291443001, 232.6198905765656377, 7.653668647301805628 ) ) ;
#18009 = EDGE_LOOP ( 'NONE', ( #12882, #16697, #6329, #18110, #6113, #5528, #9890, #5474 ) ) ;
#18010 = EDGE_CURVE ( 'NONE', #13344, #6352, #13706, .T. ) ;
#18011 = AXIS2_PLACEMENT_3D ( 'NONE', #6590, #13213, #1421 ) ;
#18012 = DIRECTION ( 'NONE',  ( -1.000000000000000000, 0.000000000000000000, 0.000000000000000000 ) ) ;
#18013 = CARTESIAN_POINT ( 'NONE',  ( -28.68588794268869790, 221.3698905683720284, -16.75240474999999307 ) ) ;
#18014 = ORIENTED_EDGE ( 'NONE', *, *, #19607, .F. ) ;
#18015 = CARTESIAN_POINT ( 'NONE',  ( -45.43829269268872650, 503.8698905683720568, 0.000000000000000000 ) ) ;
#18016 = LINE ( 'NONE', #11528, #6925 ) ;
#18017 = CARTESIAN_POINT ( 'NONE',  ( -8.685887942688729879, 437.3073905765655809, -3.978247347593165895 ) ) ;
#18018 = CARTESIAN_POINT ( 'NONE',  ( -28.68588794268870856, 299.4948905765656377, -19.99999999999999289 ) ) ;
#18019 = LINE ( 'NONE', #15012, #17519 ) ;
#18020 = DIRECTION ( 'NONE',  ( 1.854788578061058554E-16, 1.000000000000000000, 0.000000000000000000 ) ) ;
#18021 = LINE ( 'NONE', #19642, #150 ) ;
#18022 = LINE ( 'NONE', #3216, #20523 ) ;
#18023 = EDGE_CURVE ( 'NONE', #1107, #17719, #308, .T. ) ;
#18024 = LINE ( 'NONE', #19645, #5938 ) ;
#18025 = CARTESIAN_POINT ( 'NONE',  ( -48.68588794268873698, 573.2448905601785327, 0.000000000000000000 ) ) ;
#18026 = CARTESIAN_POINT ( 'NONE',  ( -13.20868407381885135, 309.7448905683720568, 6.410867750099229490 ) ) ;
#18027 = CARTESIAN_POINT ( 'NONE',  ( -8.685887942688731655, 446.9948905765655809, -2.449293598294705724E-15 ) ) ;
#18028 = CARTESIAN_POINT ( 'NONE',  ( -8.685887942688712116, 272.5573905601785327, -3.978247347593165895 ) ) ;
#18029 = CARTESIAN_POINT ( 'NONE',  ( -43.68588794268873698, 548.2448905601784190, 0.000000000000000000 ) ) ;
#18030 = MECHANICAL_DESIGN_GEOMETRIC_PRESENTATION_REPRESENTATION (  '', ( #8361 ), #11464 ) ;
#18031 = CARTESIAN_POINT ( 'NONE',  ( -19.19641293061497578, 281.9323905683720568, -14.20200298773971603 ) ) ;
#18032 = CARTESIAN_POINT ( 'NONE',  ( -45.43829269268873361, 525.0573905683720568, -3.332260488124726638 ) ) ;
#18033 = CARTESIAN_POINT ( 'NONE',  ( -45.64106924314018698, 358.1823905601784759, 11.32908994701042715 ) ) ;
#18034 = EDGE_CURVE ( 'NONE', #3413, #14255, #4023, .T. ) ;
#18035 = ORIENTED_EDGE ( 'NONE', *, *, #17994, .F. ) ;
#18036 = CARTESIAN_POINT ( 'NONE',  ( -42.88789093042844769, 484.4323905683719431, -9.489475012073736337 ) ) ;
#18037 = LINE ( 'NONE', #11228, #12851 ) ;
#18038 = CARTESIAN_POINT ( 'NONE',  ( -28.68588794268870146, 286.3698905683720568, 16.75240474999999307 ) ) ;
#18039 = VERTEX_POINT ( 'NONE', #11860 ) ;
#18040 = CARTESIAN_POINT ( 'NONE',  ( -38.17536295476244845, 293.8073905683720000, -14.20200298773971426 ) ) ;
#18041 = CARTESIAN_POINT ( 'NONE',  ( -35.09675569278793716, 311.9948905683720568, -15.47720386886985544 ) ) ;
#18042 = CIRCLE ( 'NONE', #790, 5.000000000000004441 ) ;
#18043 = CARTESIAN_POINT ( 'NONE',  ( -42.88789093042841927, 256.3073905683720568, 9.489475012073734561 ) ) ;
#18044 = ADVANCED_FACE ( 'NONE', ( #8602, #11754 ), #18455, .T. ) ;
#18045 = CARTESIAN_POINT ( 'NONE',  ( -8.685887942688708563, 247.3073905765656377, -3.978247347593165895 ) ) ;
#18046 = DIRECTION ( 'NONE',  ( 0.4627175328665442677, 0.000000000000000000, 0.8865057725575724579 ) ) ;
#18047 = CARTESIAN_POINT ( 'NONE',  ( -22.27502019258945865, 226.9948905683720284, 15.47720386886985189 ) ) ;
#18048 = CARTESIAN_POINT ( 'NONE',  ( -11.93348319268872260, 370.6823905683719431, -3.332260488124732856 ) ) ;
#18049 = DIRECTION ( 'NONE',  ( 0.3090169943749473958, 0.000000000000000000, 0.9510565162951535312 ) ) ;
#18050 = CARTESIAN_POINT ( 'NONE',  ( 91.21585410611801592, 56.85652257517427444, -85.46735025547123143 ) ) ;
#18051 = VECTOR ( 'NONE', #1380, 1000.000000000000000 ) ;
#18052 = FACE_OUTER_BOUND ( 'NONE', #7412, .T. ) ;
#18053 = CARTESIAN_POINT ( 'NONE',  ( -19.19641293061498999, 417.3073905683720568, 14.20200298773971426 ) ) ;
#18054 = DIRECTION ( 'NONE',  ( -1.191790137725560488E-16, 1.000000000000000000, -0.000000000000000000 ) ) ;
#18055 = ORIENTED_EDGE ( 'NONE', *, *, #5730, .F. ) ;
#18056 = CARTESIAN_POINT ( 'NONE',  ( -21.03221929538693047, 424.1198905601784759, -18.47759065022572855 ) ) ;
#18057 = ORIENTED_EDGE ( 'NONE', *, *, #10939, .T. ) ;
#18058 = DIRECTION ( 'NONE',  ( -1.000000000000000000, -0.000000000000000000, -0.000000000000000000 ) ) ;
#18059 = EDGE_LOOP ( 'NONE', ( #14784, #16561, #396, #15002, #2218, #5183, #10212, #20278, #4812 ) ) ;
#18060 = ORIENTED_EDGE ( 'NONE', *, *, #5380, .F. ) ;
#18061 = CARTESIAN_POINT ( 'NONE',  ( -17.35679799567829207, 313.8073905601784190, -16.95518130045146421 ) ) ;
#18062 = PLANE ( 'NONE',  #13874 ) ;
#18063 = AXIS2_PLACEMENT_3D ( 'NONE', #17298, #2482, #655 ) ;
#18064 = CARTESIAN_POINT ( 'NONE',  ( -45.43829269268871229, 335.3698905683720000, 0.000000000000000000 ) ) ;
#18065 = CARTESIAN_POINT ( 'NONE',  ( -17.35679799567830628, 475.4323905765655809, 16.95518130045146421 ) ) ;
#18066 = CARTESIAN_POINT ( 'NONE',  ( -11.93348319268872260, 359.1823905683720000, -3.332260488124732856 ) ) ;
#18067 = CARTESIAN_POINT ( 'NONE',  ( -42.82802356641965247, 310.7448905765656377, -14.14213562373094746 ) ) ;
#18068 = CARTESIAN_POINT ( 'NONE',  ( -16.84014894278199037, 387.6198905683720568, 11.84573899990672530 ) ) ;
#18069 = CARTESIAN_POINT ( 'NONE',  ( -8.685887942688717445, 316.9948905765655809, -2.449293598294705724E-15 ) ) ;
#18070 = DIRECTION ( 'NONE',  ( -1.000000000000000000, 0.000000000000000000, 0.000000000000000000 ) ) ;
#18071 = CARTESIAN_POINT ( 'NONE',  ( -35.09675569278794427, 295.7448905683720568, 15.47720386886985366 ) ) ;
#18072 = DIRECTION ( 'NONE',  ( -1.000000000000000000, 0.000000000000000000, 0.000000000000000000 ) ) ;
#18073 = ADVANCED_FACE ( 'NONE', ( #2034 ), #418, .F. ) ;
#18074 = CARTESIAN_POINT ( 'NONE',  ( -40.53162694259544452, 434.1198905683720000, -11.84573899990672707 ) ) ;
#18075 = ADVANCED_FACE ( 'NONE', ( #10329 ), #16951, .F. ) ;
#18076 = DIRECTION ( 'NONE',  ( -1.000000000000000000, -0.000000000000000000, -0.000000000000000000 ) ) ;
#18077 = CARTESIAN_POINT ( 'NONE',  ( -17.35679799567831338, 513.8073905601785327, -16.95518130045146421 ) ) ;
#18078 = DIRECTION ( 'NONE',  ( 1.000000000000000000, 0.000000000000000000, 0.000000000000000000 ) ) ;
#18079 = CARTESIAN_POINT ( 'NONE',  ( 0.000000000000000000, 0.000000000000000000, 0.000000000000000000 ) ) ;
#18080 = VECTOR ( 'NONE', #4476, 1000.000000000000000 ) ;
#18081 = CARTESIAN_POINT ( 'NONE',  ( -22.27502019258948351, 342.2448905683720568, -15.47720386886985544 ) ) ;
#18082 = CARTESIAN_POINT ( 'NONE',  ( -13.20868407381887444, 488.2448905683720000, 6.410867750099229490 ) ) ;
#18083 = AXIS2_PLACEMENT_3D ( 'NONE', #9660, #21246, #11390 ) ;
#18084 = VERTEX_POINT ( 'NONE', #523 ) ;
#18085 = CARTESIAN_POINT ( 'NONE',  ( -17.35679799567831338, 493.8073905601785327, -16.95518130045146421 ) ) ;
#18086 = CARTESIAN_POINT ( 'NONE',  ( -11.93348319268871549, 299.1823905683720000, -3.332260488124732856 ) ) ;
#18087 = ORIENTED_EDGE ( 'NONE', *, *, #1483, .T. ) ;
#18088 = CARTESIAN_POINT ( 'NONE',  ( -228.6858879426887654, 575.7448905601785327, 2.449293598294706434E-14 ) ) ;
#18089 = ORIENTED_EDGE ( 'NONE', *, *, #3737, .F. ) ;
#18090 = DIRECTION ( 'NONE',  ( -1.000000000000000000, 0.000000000000000000, 0.000000000000000000 ) ) ;
#18091 = CARTESIAN_POINT ( 'NONE',  ( -35.09675569278795138, 413.4948905683720000, -15.47720386886985544 ) ) ;
#18092 = CARTESIAN_POINT ( 'NONE',  ( -32.66413529028187668, 444.1823905765656377, 19.99999999999999289 ) ) ;
#18093 = DIRECTION ( 'NONE',  ( -1.191790137725560488E-16, 1.000000000000000000, -0.000000000000000000 ) ) ;
#18094 = CARTESIAN_POINT ( 'NONE',  ( -40.53162694259544452, 445.1198905683720568, 11.84573899990672885 ) ) ;
#18095 = CARTESIAN_POINT ( 'NONE',  ( -42.88789093042844058, 444.8073905683720568, 9.489475012073734561 ) ) ;
#18096 = PRODUCT_CONTEXT ( 'NONE', #17977, 'mechanical' ) ;
#18097 = DIRECTION ( 'NONE',  ( -0.000000000000000000, -0.000000000000000000, 1.000000000000000000 ) ) ;
#18098 = CARTESIAN_POINT ( 'NONE',  ( -8.685887942688724550, 376.9948905765655809, -2.449293598294705724E-15 ) ) ;
#18099 = DIRECTION ( 'NONE',  ( -1.000000000000000000, 0.000000000000000000, -0.000000000000000000 ) ) ;
#18100 = CARTESIAN_POINT ( 'NONE',  ( -45.64106924314016567, 266.3073905601784190, -11.32908994701042538 ) ) ;
#18101 = LINE ( 'NONE', #6628, #8758 ) ;
#18102 = CARTESIAN_POINT ( 'NONE',  ( 60.03793209889851568, 30.52886280891152282, 131.1729372809869005 ) ) ;
#18103 = CONICAL_SURFACE ( 'NONE', #8774, 6.500000000000000000, 1.047197551196600296 ) ;
#18104 = CARTESIAN_POINT ( 'NONE',  ( -35.09675569278796559, 487.2448905683720000, 15.47720386886985366 ) ) ;
#18105 = DIRECTION ( 'NONE',  ( -1.000000000000000000, 0.000000000000000000, 0.000000000000000000 ) ) ;
#18106 = CARTESIAN_POINT ( 'NONE',  ( -11.73070664223726567, 521.3073905601785327, 11.32908994701042005 ) ) ;
#18107 = CARTESIAN_POINT ( 'NONE',  ( -44.16309181155857999, 404.7448905683720568, -6.410867750099231266 ) ) ;
#18108 = CARTESIAN_POINT ( 'NONE',  ( 20.22541975382790369, 160.1716627696692683, 61.32575462769902686 ) ) ;
#18109 = CARTESIAN_POINT ( 'NONE',  ( -45.43829269268869098, 225.6823905683720568, 3.332260488124734632 ) ) ;
#18110 = ORIENTED_EDGE ( 'NONE', *, *, #18733, .T. ) ;
#18111 = CARTESIAN_POINT ( 'NONE',  ( -28.68588794268874054, 573.2448905601785327, 0.000000000000000000 ) ) ;
#18112 = ORIENTED_EDGE ( 'NONE', *, *, #17042, .F. ) ;
#18113 = CARTESIAN_POINT ( 'NONE',  ( -44.16309181155857999, 444.7448905683720000, -6.410867750099231266 ) ) ;
#18114 = CARTESIAN_POINT ( 'NONE',  ( -38.17536295476246977, 525.4323905683720568, 14.20200298773971781 ) ) ;
#18115 = ORIENTED_EDGE ( 'NONE', *, *, #9361, .F. ) ;
#18116 = FACE_OUTER_BOUND ( 'NONE', #6090, .T. ) ;
#18117 = CARTESIAN_POINT ( 'NONE',  ( -16.84014894278196905, 227.6198905683720000, 11.84573899990672530 ) ) ;
#18118 = VERTEX_POINT ( 'NONE', #2661 ) ;
#18119 = EDGE_CURVE ( 'NONE', #451, #1584, #10867, .T. ) ;
#18120 = CARTESIAN_POINT ( 'NONE',  ( -42.88789093042845479, 512.9323905683720568, -9.489475012073734561 ) ) ;
#18121 = CARTESIAN_POINT ( 'NONE',  ( 0.000000000000000000, 5.629165124598846326, -3.250000000000007550 ) ) ;
#18122 = CARTESIAN_POINT ( 'NONE',  ( -17.35679799567830983, 438.5573905765655809, -16.95518130045146421 ) ) ;
#18123 = DIRECTION ( 'NONE',  ( -1.191790137725560488E-16, 1.000000000000000000, 0.000000000000000000 ) ) ;
#18124 = EDGE_CURVE ( 'NONE', #8857, #8848, #12932, .T. ) ;
#18125 = CARTESIAN_POINT ( 'NONE',  ( 30.42502041961814285, 230.5765313837437418, 40.00000000000000000 ) ) ;
#18126 = CARTESIAN_POINT ( 'NONE',  ( -36.33955658999052929, 453.8698905765656377, 18.47759065022572500 ) ) ;
#18127 = DIRECTION ( 'NONE',  ( 0.000000000000000000, 0.000000000000000000, 1.000000000000000000 ) ) ;
#18128 = CARTESIAN_POINT ( 'NONE',  ( -17.35679799567828141, 290.6823905601785327, 16.95518130045146421 ) ) ;
#18129 = DIRECTION ( 'NONE',  ( 0.000000000000000000, 0.000000000000000000, 1.000000000000000000 ) ) ;
#18130 = CARTESIAN_POINT ( 'NONE',  ( -17.35679799567830628, 495.4323905765656946, 16.95518130045146421 ) ) ;
#18131 = CARTESIAN_POINT ( 'NONE',  ( -42.88789093042842637, 314.4323905683720000, -9.489475012073736337 ) ) ;
#18132 = CARTESIAN_POINT ( 'NONE',  ( -40.01497788969912506, 235.6823905601784759, -16.95518130045146421 ) ) ;
#18133 = CARTESIAN_POINT ( 'NONE',  ( -24.70764059509553334, 260.0573905601784190, 19.99999999999998934 ) ) ;
#18134 = CARTESIAN_POINT ( 'NONE',  ( -10.76731745429009912, 56.85652257517428865, -118.3724535612433328 ) ) ;
#18135 = CARTESIAN_POINT ( 'NONE',  ( -28.68588794268870501, 297.8698905683720000, 16.75240474999999307 ) ) ;
#18136 = CARTESIAN_POINT ( 'NONE',  ( -25.35362745456399836, 508.1823905683720000, 16.75240474999998952 ) ) ;
#18137 = CARTESIAN_POINT ( 'NONE',  ( -36.33955658999050797, 375.3698905601784759, -18.47759065022572855 ) ) ;
#18138 = EDGE_CURVE ( 'NONE', #763, #9302, #20403, .T. ) ;
#18139 = DIRECTION ( 'NONE',  ( 0.000000000000000000, 0.000000000000000000, 1.000000000000000000 ) ) ;
#18140 = EDGE_LOOP ( 'NONE', ( #2856, #9831 ) ) ;
#18141 = CARTESIAN_POINT ( 'NONE',  ( -38.17536295476246266, 476.9323905683720568, 14.20200298773971781 ) ) ;
#18142 = CARTESIAN_POINT ( 'NONE',  ( -40.53162694259543031, 282.6198905683720000, -11.84573899990672707 ) ) ;
#18143 = VERTEX_POINT ( 'NONE', #20514 ) ;
#18144 = DIRECTION ( 'NONE',  ( 0.000000000000000000, -1.000000000000000000, 0.000000000000000000 ) ) ;
#18145 = CARTESIAN_POINT ( 'NONE',  ( -14.48388495494899075, 291.3073905683720568, -9.489475012073734561 ) ) ;
#18146 = CARTESIAN_POINT ( 'NONE',  ( -36.33955658999049376, 240.1198905765656377, -18.47759065022572855 ) ) ;
#18147 = CARTESIAN_POINT ( 'NONE',  ( -21.03221929538693047, 418.8698905765655809, -18.47759065022572855 ) ) ;
#18148 = FACE_OUTER_BOUND ( 'NONE', #11406, .T. ) ;
#18149 = CARTESIAN_POINT ( 'NONE',  ( -35.09675569278793716, 271.9948905683720000, -15.47720386886985544 ) ) ;
#18150 = CARTESIAN_POINT ( 'NONE',  ( -35.09675569278794427, 373.4948905683720568, -15.47720386886985544 ) ) ;
#18151 = EDGE_CURVE ( 'NONE', #4289, #11401, #2556, .T. ) ;
#18152 = CARTESIAN_POINT ( 'NONE',  ( -43.68588794268870146, 200.1437886375729249, 0.3330356950053358633 ) ) ;
#18153 = CARTESIAN_POINT ( 'NONE',  ( -11.73070664223726212, 457.9323905765655809, -11.32908994701042538 ) ) ;
#18154 =( BOUNDED_CURVE ( )  B_SPLINE_CURVE ( 3, ( #8604, #4944, #11543, #18134 ),
 .UNSPECIFIED., .F., .T. ) 
 B_SPLINE_CURVE_WITH_KNOTS ( ( 4, 4 ),
 ( 4.712388980384691450, 6.283185307179586232 ),
 .UNSPECIFIED. ) 
 CURVE ( )  GEOMETRIC_REPRESENTATION_ITEM ( )  RATIONAL_B_SPLINE_CURVE ( ( 1.000000000000000000, 0.8047378541243654926, 0.8047378541243654926, 1.000000000000000000 ) ) 
 REPRESENTATION_ITEM ( '' )  );
#18155 = CARTESIAN_POINT ( 'NONE',  ( -28.68588794268870501, 269.4948905765656377, -19.99999999999999289 ) ) ;
#18156 = CARTESIAN_POINT ( 'NONE',  ( -19.19641293061498999, 420.4323905683720000, -14.20200298773971603 ) ) ;
#18157 = LINE ( 'NONE', #11990, #5699 ) ;
#18158 = ORIENTED_EDGE ( 'NONE', *, *, #38, .T. ) ;
#18159 = CARTESIAN_POINT ( 'NONE',  ( -10.20829729246299422, 431.6198905601785327, 7.653668647301790529 ) ) ;
#18160 = EDGE_CURVE ( 'NONE', #4322, #11378, #19549, .T. ) ;
#18161 = ORIENTED_EDGE ( 'NONE', *, *, #5872, .F. ) ;
#18162 = DIRECTION ( 'NONE',  ( 0.000000000000000000, 0.000000000000000000, 1.000000000000000000 ) ) ;
#18163 = VERTEX_POINT ( 'NONE', #9032 ) ;
#18164 = VERTEX_POINT ( 'NONE', #7190 ) ;
#18165 = DIRECTION ( 'NONE',  ( -0.000000000000000000, 1.000000000000000000, 1.155626614413199331E-16 ) ) ;
#18166 = CARTESIAN_POINT ( 'NONE',  ( -48.68588794268870146, 296.9323905601784759, -3.978247347593158345 ) ) ;
#18167 = CYLINDRICAL_SURFACE ( 'NONE', #4554, 210.7252770684331438 ) ;
#18168 = CARTESIAN_POINT ( 'NONE',  ( -11.93348319268871904, 350.3698905683720568, -2.051577885510841163E-15 ) ) ;
#18169 = VERTEX_POINT ( 'NONE', #1055 ) ;
#18170 = CARTESIAN_POINT ( 'NONE',  ( -10.20829729246300133, 486.3698905765655809, 7.653668647301790529 ) ) ;
#18171 = CARTESIAN_POINT ( 'NONE',  ( -14.48388495494899963, 367.9323905683720000, 9.489475012073732785 ) ) ;
#18172 = CARTESIAN_POINT ( 'NONE',  ( 0.4033376246892473871, 4.059728990630799395, 5.968343123267132455 ) ) ;
#18173 = CARTESIAN_POINT ( 'NONE',  ( -42.88789093042843348, 384.8073905683720568, 9.489475012073734561 ) ) ;
#18174 = AXIS2_PLACEMENT_3D ( 'NONE', #14006, #7161, #7380 ) ;
#18175 = CARTESIAN_POINT ( 'NONE',  ( -8.685887942688715668, 296.9948905765655809, -2.449293598294705724E-15 ) ) ;
#18176 = DIRECTION ( 'NONE',  ( 0.000000000000000000, 0.000000000000000000, 1.000000000000000000 ) ) ;
#18177 = CARTESIAN_POINT ( 'NONE',  ( -14.48388495494899075, 289.8073905683719431, -9.489475012073734561 ) ) ;
#18178 = FACE_OUTER_BOUND ( 'NONE', #18335, .T. ) ;
#18179 = CARTESIAN_POINT ( 'NONE',  ( -28.68588794268872633, 442.8698905683720568, -16.75240474999999307 ) ) ;
#18180 = CONICAL_SURFACE ( 'NONE', #8847, 6.500000000000000000, 1.047197551196600296 ) ;
#18181 = PLANE ( 'NONE',  #15465 ) ;
#18182 = CARTESIAN_POINT ( 'NONE',  ( -47.16347859291446554, 516.6198905601784190, -7.653668647301793193 ) ) ;
#18183 = CARTESIAN_POINT ( 'NONE',  ( 0.2595206531158515961, 2.531175536751804955, -6.499999999999999112 ) ) ;
#18184 = DIRECTION ( 'NONE',  ( 0.000000000000000000, 0.000000000000000000, 1.000000000000000000 ) ) ;
#18185 = CARTESIAN_POINT ( 'NONE',  ( -40.53162694259543741, 346.6198905683720000, 11.84573899990672885 ) ) ;
#18186 = CARTESIAN_POINT ( 'NONE',  ( -44.16309181155857999, 474.4948905683720000, 6.410867750099241924 ) ) ;
#18187 = EDGE_LOOP ( 'NONE', ( #5340, #13444, #7072, #8452 ) ) ;
#18188 = CARTESIAN_POINT ( 'NONE',  ( -47.16347859291445843, 496.6198905601784759, -7.653668647301793193 ) ) ;
#18189 = CARTESIAN_POINT ( 'NONE',  ( -38.17536295476244135, 305.4323905683720000, 14.20200298773971781 ) ) ;
#18190 = ORIENTED_EDGE ( 'NONE', *, *, #730, .F. ) ;
#18191 = EDGE_LOOP ( 'NONE', ( #5388, #430, #9992, #2167, #11195, #2935, #155 ) ) ;
#18192 = DIRECTION ( 'NONE',  ( 1.000000000000000000, 0.000000000000000000, 0.000000000000000000 ) ) ;
#18193 = ADVANCED_FACE ( 'NONE', ( #14248 ), #9138, .F. ) ;
#18194 = CIRCLE ( 'NONE', #8866, 175.0000000000000284 ) ;
#18195 = CARTESIAN_POINT ( 'NONE',  ( -44.16309181155857999, 394.7448905683720568, -6.410867750099231266 ) ) ;
#18196 = PLANE ( 'NONE',  #20757 ) ;
#18197 = FILL_AREA_STYLE ('',( #6732 ) ) ;
#18198 = CARTESIAN_POINT ( 'NONE',  ( -19.19641293061498999, 430.4323905683720000, -14.20200298773971603 ) ) ;
#18199 = CARTESIAN_POINT ( 'NONE',  ( -35.09675569278795848, 451.9948905683720000, -15.47720386886985544 ) ) ;
#18200 =( NAMED_UNIT ( * ) SI_UNIT ( $, .STERADIAN. ) SOLID_ANGLE_UNIT ( ) );
#18201 = LINE ( 'NONE', #1896, #9967 ) ;
#18202 = CARTESIAN_POINT ( 'NONE',  ( -21.03221929538692336, 368.8698905765656377, -18.47759065022572855 ) ) ;
#18203 = CARTESIAN_POINT ( 'NONE',  ( -10.76731745429010267, 56.32691141864442841, 46.25122601329427852 ) ) ;
#18204 = FACE_OUTER_BOUND ( 'NONE', #9168, .T. ) ;
#18205 = FACE_OUTER_BOUND ( 'NONE', #7226, .T. ) ;
#18206 = DIRECTION ( 'NONE',  ( 0.9365583756827543516, -0.000000000000000000, -0.3505116388060184329 ) ) ;
#18207 = CARTESIAN_POINT ( 'NONE',  ( -32.01814843081346140, 493.1823905683721136, -16.75240474999999307 ) ) ;
#18208 = ADVANCED_FACE ( 'NONE', ( #7407 ), #14033, .T. ) ;
#18209 = CIRCLE ( 'NONE', #16498, 125.0000000000000000 ) ;
#18210 = PLANE ( 'NONE',  #15453 ) ;
#18211 = DIRECTION ( 'NONE',  ( 1.191790137725560488E-16, -1.000000000000000000, -0.000000000000000000 ) ) ;
#18212 = CARTESIAN_POINT ( 'NONE',  ( -24.70764059509556532, 520.0573905601784190, 19.99999999999998934 ) ) ;
#18213 = EDGE_CURVE ( 'NONE', #13873, #8747, #20613, .T. ) ;
#18214 = EDGE_CURVE ( 'NONE', #5669, #13344, #19558, .T. ) ;
#18215 = CIRCLE ( 'NONE', #8542, 4.000000000000003553 ) ;
#18216 = CARTESIAN_POINT ( 'NONE',  ( -32.01814843081345430, 397.5573905683721136, 16.75240474999999307 ) ) ;
#18217 = CARTESIAN_POINT ( 'NONE',  ( -45.64106924314016567, 262.9323905765656377, 11.32908994701042538 ) ) ;
#18218 = CARTESIAN_POINT ( 'NONE',  ( -25.35362745456396638, 238.1823905683720852, 16.75240474999998952 ) ) ;
#18219 = CARTESIAN_POINT ( 'NONE',  ( -22.27502019258948707, 360.7448905683720568, -15.47720386886985544 ) ) ;
#18220 = EDGE_LOOP ( 'NONE', ( #13209, #5953, #11677, #295, #20226, #3461, #15393, #1667, #19736, #4835, #2491, #17740, #15919, #19745, #10679, #6615, #746, #15051, #9414, #9256, #1744, #7393, #11139, #14068, #8504, #20307, #15918, #10923, #1060, #10949, #18638, #4979, #1740, #17477, #13743, #10797, #9363, #17413, #12486, #20098, #12980, #4214, #5636, #10556, #18748, #7628, #853, #15495, #11844, #17010, #12917, #20914, #5737, #6212, #16451, #9174, #10134, #20178, #11740, #16724, #76, #12132, #19139, #7969, #737, #7548 ) ) ;
#18221 = CARTESIAN_POINT ( 'NONE',  ( -25.35362745456401257, 521.0573905683720568, -16.75240474999999307 ) ) ;
#18222 = ORIENTED_EDGE ( 'NONE', *, *, #16505, .T. ) ;
#18223 = CARTESIAN_POINT ( 'NONE',  ( -25.35362745456400191, 442.5573905683720568, -16.75240474999999307 ) ) ;
#18224 = CARTESIAN_POINT ( 'NONE',  ( -13.20868407381888154, 529.4948905683720568, -6.410867750099233042 ) ) ;
#18225 = EDGE_CURVE ( 'NONE', #14938, #2589, #20936, .T. ) ;
#18226 = ORIENTED_EDGE ( 'NONE', *, *, #11483, .F. ) ;
#18227 = CARTESIAN_POINT ( 'NONE',  ( -42.82802356641966668, 428.4948905601784759, 14.14213562373094923 ) ) ;
#18228 = CARTESIAN_POINT ( 'NONE',  ( -35.09675569278796559, 475.7448905683720568, 15.47720386886985366 ) ) ;
#18229 = EDGE_LOOP ( 'NONE', ( #17840, #3388, #18406, #11242, #20544, #6507 ) ) ;
#18230 = CARTESIAN_POINT ( 'NONE',  ( -19.19641293061499709, 507.3073905683720568, 14.20200298773971426 ) ) ;
#18231 = CARTESIAN_POINT ( 'NONE',  ( -14.71623956875115447, 48.14959005838937145, -47.59463164328435170 ) ) ;
#18232 = CARTESIAN_POINT ( 'NONE',  ( -47.16347859291445133, 442.6198905765656377, 7.653668647301805628 ) ) ;
#18233 = CARTESIAN_POINT ( 'NONE',  ( -21.03221929538692336, 358.8698905765656377, -18.47759065022572855 ) ) ;
#18234 = CARTESIAN_POINT ( 'NONE',  ( -47.16347859291443712, 327.8698905601785327, 7.653668647301805628 ) ) ;
#18235 = DIRECTION ( 'NONE',  ( -1.191790137725560488E-16, 1.000000000000000000, -0.000000000000000000 ) ) ;
#18236 = CARTESIAN_POINT ( 'NONE',  ( 28.16023193154655502, 323.8848358243226357, 20.00000000000000355 ) ) ;
#18237 = LINE ( 'NONE', #18346, #21213 ) ;
#18238 = DIRECTION ( 'NONE',  ( -0.000000000000000000, -1.000000000000000000, -0.000000000000000000 ) ) ;
#18239 = CARTESIAN_POINT ( 'NONE',  ( -43.47648769733579854, 200.8087914445877971, -2.512805286998617049 ) ) ;
#18240 = CARTESIAN_POINT ( 'NONE',  ( -35.09675569278793716, 303.4948905683720568, -15.47720386886985544 ) ) ;
#18241 = DIRECTION ( 'NONE',  ( -1.000000000000000000, 0.000000000000000000, 0.000000000000000000 ) ) ;
#18242 = CARTESIAN_POINT ( 'NONE',  ( -47.16347859291443001, 267.8698905601784759, 7.653668647301805628 ) ) ;
#18243 = CARTESIAN_POINT ( 'NONE',  ( 40.42502041961814996, 180.1716627696692967, 20.00000000000000355 ) ) ;
#18244 = CARTESIAN_POINT ( 'NONE',  ( -11.93348319268871194, 290.3698905683720568, -2.051577885510841163E-15 ) ) ;
#18245 = CARTESIAN_POINT ( 'NONE',  ( 14.09825962131072785, 230.5765313837437418, 49.99999999999999289 ) ) ;
#18246 = CARTESIAN_POINT ( 'NONE',  ( -13.20868407381887799, 510.9948905683721136, -6.410867750099233042 ) ) ;
#18247 = CARTESIAN_POINT ( 'NONE',  ( -15.54750367907771746, 45.31613216062294214, 120.2864949470673110 ) ) ;
#18248 = ORIENTED_EDGE ( 'NONE', *, *, #1000, .T. ) ;
#18249 = CARTESIAN_POINT ( 'NONE',  ( -45.43829269268872650, 465.3698905683720000, 0.000000000000000000 ) ) ;
#18250 = CARTESIAN_POINT ( 'NONE',  ( -8.685887942688717445, 316.9948905765655809, -2.449293598294705724E-15 ) ) ;
#18251 = CARTESIAN_POINT ( 'NONE',  ( -45.43829269268869098, 264.1823905683720000, 3.332260488124734632 ) ) ;
#18252 = ORIENTED_EDGE ( 'NONE', *, *, #3102, .T. ) ;
#18253 = DIRECTION ( 'NONE',  ( -1.191790137725560488E-16, 1.000000000000000000, -0.000000000000000000 ) ) ;
#18254 = AXIS2_PLACEMENT_3D ( 'NONE', #13696, #10429, #15117 ) ;
#18255 = CARTESIAN_POINT ( 'NONE',  ( -44.16309181155855867, 264.7448905683720000, -6.410867750099231266 ) ) ;
#18256 = CARTESIAN_POINT ( 'NONE',  ( -32.66413529028186247, 244.1823905765655809, 19.99999999999999289 ) ) ;
#18257 = DIRECTION ( 'NONE',  ( 0.000000000000000000, -1.155626614413199331E-16, 1.000000000000000000 ) ) ;
#18258 = CARTESIAN_POINT ( 'NONE',  ( -14.54375231895775400, 233.4948905601784759, -14.14213562373094746 ) ) ;
#18259 = CARTESIAN_POINT ( 'NONE',  ( -24.70764059509554755, 259.1823905765656377, -19.99999999999999289 ) ) ;
#18260 = CARTESIAN_POINT ( 'NONE',  ( -22.27502019258946575, 266.9948905683720000, 15.47720386886985189 ) ) ;
#18261 = CARTESIAN_POINT ( 'NONE',  ( -16.84014894278199037, 351.6198905683720000, -11.84573899990672707 ) ) ;
#18262 = EDGE_CURVE ( 'NONE', #15902, #16993, #9184, .T. ) ;
#18263 = DIRECTION ( 'NONE',  ( -0.000000000000000000, -1.000000000000000000, -0.000000000000000000 ) ) ;
#18264 = DIRECTION ( 'NONE',  ( -1.000000000000000000, -0.000000000000000000, -0.000000000000000000 ) ) ;
#18265 = VECTOR ( 'NONE', #6599, 1000.000000000000000 ) ;
#18266 = CARTESIAN_POINT ( 'NONE',  ( -38.17536295476245556, 425.4323905683720000, 14.20200298773971781 ) ) ;
#18267 = ORIENTED_EDGE ( 'NONE', *, *, #17894, .T. ) ;
#18268 = CARTESIAN_POINT ( 'NONE',  ( -11.73070664223725323, 421.3073905601784190, 11.32908994701042005 ) ) ;
#18269 = ORIENTED_EDGE ( 'NONE', *, *, #6260, .T. ) ;
#18270 = CARTESIAN_POINT ( 'NONE',  ( 0.4033376246892497741, 7.198601258566900363, -0.5316568767328673228 ) ) ;
#18271 = ORIENTED_EDGE ( 'NONE', *, *, #8244, .T. ) ;
#18272 = EDGE_LOOP ( 'NONE', ( #19313, #12102 ) ) ;
#18273 = CARTESIAN_POINT ( 'NONE',  ( -42.88789093042845479, 524.4323905683720568, -9.489475012073736337 ) ) ;
#18274 = CARTESIAN_POINT ( 'NONE',  ( -8.685887942688715668, 302.2448905601784190, -2.449293598294705724E-15 ) ) ;
#18275 = DIRECTION ( 'NONE',  ( -1.000000000000000000, -0.000000000000000000, -0.000000000000000000 ) ) ;
#18276 = EDGE_CURVE ( 'NONE', #8381, #11550, #19816, .T. ) ;
#18277 = CARTESIAN_POINT ( 'NONE',  ( -35.09675569278793716, 323.4948905683720000, -15.47720386886985544 ) ) ;
#18278 = ORIENTED_EDGE ( 'NONE', *, *, #18866, .F. ) ;
#18279 = CARTESIAN_POINT ( 'NONE',  ( -42.82802356641967378, 483.2448905765656377, 14.14213562373094923 ) ) ;
#18280 = CARTESIAN_POINT ( 'NONE',  ( -13.20868407381886200, 369.4948905683720568, -6.410867750099233042 ) ) ;
#18281 = CARTESIAN_POINT ( 'NONE',  ( -40.53162694259543741, 362.6198905683720000, -11.84573899990672707 ) ) ;
#18282 = VECTOR ( 'NONE', #7233, 1000.000000000000000 ) ;
#18283 = CARTESIAN_POINT ( 'NONE',  ( -10.20829729246298001, 307.6198905765656377, -7.653668647301794969 ) ) ;
#18284 = DIRECTION ( 'NONE',  ( -0.000000000000000000, 1.000000000000000000, -0.000000000000000000 ) ) ;
#18285 = CARTESIAN_POINT ( 'NONE',  ( -38.17536295476244135, 275.4323905683720568, 14.20200298773971781 ) ) ;
#18286 = CARTESIAN_POINT ( 'NONE',  ( -28.68588794268874054, 573.2448905601785327, 0.000000000000000000 ) ) ;
#18287 =( BOUNDED_CURVE ( )  B_SPLINE_CURVE ( 2, ( #17196, #12216, #7329, #5389, #15369, #8849, #9065, #13960, #10359, #19024, #13841, #2165, #11995, #8748, #20545, #5711, #5498 ),
 .UNSPECIFIED., .F., .T. ) 
 B_SPLINE_CURVE_WITH_KNOTS ( ( 3, 2, 2, 2, 2, 2, 2, 2, 3 ),
 ( 0.5625000000000001110, 0.5644531250000001110, 0.5664062500000001110, 0.5683593750000001110, 0.5703125000000001110, 0.5722656250000001110, 0.5742187500000001110, 0.5761718750000001110, 0.5781250000000001110 ),
 .UNSPECIFIED. ) 
 CURVE ( )  GEOMETRIC_REPRESENTATION_ITEM ( )  RATIONAL_B_SPLINE_CURVE ( ( 0.9999999999999988898, 0.9807852804032315408, 1.000000000000000000, 0.9807852804032304306, 1.000000000000000000, 0.9807852804032304306, 1.000000000000000000, 0.9807852804032304306, 1.000000000000000000, 0.9807852804032304306, 1.000000000000000000, 0.9807852804032304306, 1.000000000000000000, 0.9807852804032304306, 1.000000000000000000, 0.9807852804032293204, 1.000000000000001110 ) ) 
 REPRESENTATION_ITEM ( '' )  );
#18288 = CARTESIAN_POINT ( 'NONE',  ( -42.88789093042844058, 424.4323905683720568, -9.489475012073736337 ) ) ;
#18289 = EDGE_CURVE ( 'NONE', #6118, #6933, #2309, .T. ) ;
#18290 = CARTESIAN_POINT ( 'NONE',  ( -8.685887942688742314, 573.2448905601785327, 2.449293598294706119E-15 ) ) ;
#18291 = CARTESIAN_POINT ( 'NONE',  ( -40.01497788969916058, 515.6823905601785327, -16.95518130045146421 ) ) ;
#18292 = DIRECTION ( 'NONE',  ( -1.191790137725560488E-16, 1.000000000000000000, -0.000000000000000000 ) ) ;
#18293 = CARTESIAN_POINT ( 'NONE',  ( 4.700000000000000178, -7.505553499465150047, 0.000000000000000000 ) ) ;
#18294 = CARTESIAN_POINT ( 'NONE',  ( -45.43829269268871229, 335.3698905683720000, 0.000000000000000000 ) ) ;
#18295 = CARTESIAN_POINT ( 'NONE',  ( -25.35362745456400546, 481.0573905683720568, -16.75240474999999307 ) ) ;
#18296 = VERTEX_POINT ( 'NONE', #6606 ) ;
#18297 = CARTESIAN_POINT ( 'NONE',  ( -11.73070664223726389, 483.1823905601784759, -11.32908994701042715 ) ) ;
#18298 = CARTESIAN_POINT ( 'NONE',  ( -32.01814843081344009, 296.0573905683720000, 16.75240474999999307 ) ) ;
#18299 = VERTEX_POINT ( 'NONE', #146 ) ;
#18300 = DIRECTION ( 'NONE',  ( -1.000000000000000000, -0.000000000000000000, -0.000000000000000000 ) ) ;
#18301 = ORIENTED_EDGE ( 'NONE', *, *, #4761, .T. ) ;
#18302 = DIRECTION ( 'NONE',  ( 1.000000000000000000, 0.000000000000000000, 0.000000000000000000 ) ) ;
#18303 = CARTESIAN_POINT ( 'NONE',  ( -40.53162694259544452, 406.6198905683720568, 11.84573899990672885 ) ) ;
#18304 = CARTESIAN_POINT ( 'NONE',  ( -8.685887942688735208, 482.2448905601784759, -2.449293598294705724E-15 ) ) ;
#18305 = CARTESIAN_POINT ( 'NONE',  ( -28.68588794268874054, 573.2448905601785327, 0.000000000000000000 ) ) ;
#18306 = CARTESIAN_POINT ( 'NONE',  ( -28.68588794268872277, 421.3698905683720568, -16.75240474999999307 ) ) ;
#18307 = CARTESIAN_POINT ( 'NONE',  ( -14.48388495494898720, 269.4323905683720568, 9.489475012073732785 ) ) ;
#18308 = CARTESIAN_POINT ( 'NONE',  ( -28.68588794268872277, 436.3698905683720000, 16.75240474999999307 ) ) ;
#18309 = APPLICATION_PROTOCOL_DEFINITION ( 'draft international standard', 'automotive_design', 1998, #20777 ) ;
#18310 = DIRECTION ( 'NONE',  ( 0.000000000000000000, 0.000000000000000000, -1.000000000000000000 ) ) ;
#18311 = CARTESIAN_POINT ( 'NONE',  ( -14.54375231895776821, 365.7448905765656377, 14.14213562373094568 ) ) ;
#18312 = CARTESIAN_POINT ( 'NONE',  ( -10.20829729246297646, 272.8698905601784759, -7.653668647301794969 ) ) ;
#18313 = CARTESIAN_POINT ( 'NONE',  ( -14.54375231895775755, 263.4948905601784759, -14.14213562373094746 ) ) ;
#18314 = CARTESIAN_POINT ( 'NONE',  ( -16.84014894278198682, 330.1198905683720568, -11.84573899990672707 ) ) ;
#18315 = DIRECTION ( 'NONE',  ( 0.000000000000000000, 0.000000000000000000, -1.000000000000000000 ) ) ;
#18316 = CARTESIAN_POINT ( 'NONE',  ( -44.16309181155858710, 494.7448905683720000, -6.410867750099231266 ) ) ;
#18318 = LINE ( 'NONE', #21144, #8167 ) ;
#18317 = VECTOR ( 'NONE', #4909, 1000.000000000000114 ) ;
#18319 = DIRECTION ( 'NONE',  ( 0.000000000000000000, -1.000000000000000000, 0.000000000000000000 ) ) ;
#18320 = CARTESIAN_POINT ( 'NONE',  ( -43.60140439023965797, 209.8858117899327169, 1.618481238659645882 ) ) ;
#18321 = CARTESIAN_POINT ( 'NONE',  ( -13.20868407381886378, 399.7448905683720568, 6.410867750099229490 ) ) ;
#18322 = CARTESIAN_POINT ( 'NONE',  ( 0.000000000000000000, 0.000000000000000000, 0.000000000000000000 ) ) ;
#18323 = CARTESIAN_POINT ( 'NONE',  ( -42.88789093042841927, 226.3073905683720000, 9.489475012073736337 ) ) ;
#18324 = CARTESIAN_POINT ( 'NONE',  ( -28.68588794268871567, 371.3698905683720568, -16.75240474999999307 ) ) ;
#18325 = VERTEX_POINT ( 'NONE', #1544 ) ;
#18326 = CARTESIAN_POINT ( 'NONE',  ( -11.93348319268874036, 518.8698905683719431, -2.051577885510841163E-15 ) ) ;
#18327 = VERTEX_POINT ( 'NONE', #8115 ) ;
#18328 = CARTESIAN_POINT ( 'NONE',  ( -28.68588794268872633, 452.8698905683720000, -16.75240474999999307 ) ) ;
#18329 = CARTESIAN_POINT ( 'NONE',  ( -35.09675569278797269, 515.7448905683720568, 15.47720386886985366 ) ) ;
#18330 = ORIENTED_EDGE ( 'NONE', *, *, #19661, .F. ) ;
#18331 = CARTESIAN_POINT ( 'NONE',  ( -11.06088464903280233, 135.1716627696692683, -5.773301668816269938 ) ) ;
#18332 = CARTESIAN_POINT ( 'NONE',  ( -32.66413529028189089, 529.8073905765656946, -19.99999999999999289 ) ) ;
#18333 = CARTESIAN_POINT ( 'NONE',  ( -19.19641293061500065, 490.4323905683720000, -14.20200298773971603 ) ) ;
#18334 = ADVANCED_FACE ( 'NONE', ( #14748 ), #16827, .T. ) ;
#18335 = EDGE_LOOP ( 'NONE', ( #16028, #4971, #8432, #1109, #12047, #8702 ) ) ;
#18336 = CARTESIAN_POINT ( 'NONE',  ( -45.43829269268873361, 513.8698905683720568, 0.000000000000000000 ) ) ;
#18337 = ADVANCED_FACE ( 'NONE', ( #19205 ), #1157, .T. ) ;
#18338 = CARTESIAN_POINT ( 'NONE',  ( -45.64106924314019409, 488.1823905601784759, 11.32908994701042538 ) ) ;
#18339 = CIRCLE ( 'NONE', #7963, 49.60091809715359545 ) ;
#18341 = CIRCLE ( 'NONE', #15594, 125.0000000000000000 ) ;
#18340 = CARTESIAN_POINT ( 'NONE',  ( -40.01497788969913927, 433.5573905765656377, 16.95518130045146776 ) ) ;
#18342 = CARTESIAN_POINT ( 'NONE',  ( -40.01497788969913927, 360.4323905765656946, -16.95518130045146421 ) ) ;
#18343 = DIRECTION ( 'NONE',  ( -0.000000000000000000, -0.000000000000000000, 1.000000000000000000 ) ) ;
#18344 = DIRECTION ( 'NONE',  ( 1.000000000000000000, 0.000000000000000000, -0.000000000000000000 ) ) ;
#18345 = DIRECTION ( 'NONE',  ( 0.000000000000000000, 0.000000000000000000, 1.000000000000000000 ) ) ;
#18346 = CARTESIAN_POINT ( 'NONE',  ( 91.21585410611801592, 56.85652257517428865, 94.99999999999994316 ) ) ;
#18347 = FACE_OUTER_BOUND ( 'NONE', #9390, .T. ) ;
#18348 = CARTESIAN_POINT ( 'NONE',  ( -13.30084729135444377, 223.9102039777116886, -12.89731357292796510 ) ) ;
#18349 = CARTESIAN_POINT ( 'NONE',  ( -19.19641293061497578, 288.8073905683719431, 14.20200298773971426 ) ) ;
#18350 = EDGE_CURVE ( 'NONE', #20033, #763, #14960, .T. ) ;
#18351 = CARTESIAN_POINT ( 'NONE',  ( -8.685887942689042518, 531.9323905601784190, 3.978247347593879546 ) ) ;
#18352 = CARTESIAN_POINT ( 'NONE',  ( -45.64106924314017988, 278.1823905601784759, 11.32908994701042715 ) ) ;
#18353 = CARTESIAN_POINT ( 'NONE',  ( -21.03221929538691626, 415.1198905765656377, 18.47759065022572500 ) ) ;
#18354 = ORIENTED_EDGE ( 'NONE', *, *, #16903, .F. ) ;
#18355 = CARTESIAN_POINT ( 'NONE',  ( -47.16347859291446554, 536.6198905601784190, -7.653668647301793193 ) ) ;
#18356 = CARTESIAN_POINT ( 'NONE',  ( -16.84014894278200813, 511.6198905683720000, -11.84573899990672707 ) ) ;
#18357 = ORIENTED_EDGE ( 'NONE', *, *, #11209, .F. ) ;
#18358 = CARTESIAN_POINT ( 'NONE',  ( -44.16309181155858710, 464.7448905683720568, -6.410867750099231266 ) ) ;
#18359 = CARTESIAN_POINT ( 'NONE',  ( -10.20829729246299067, 407.6198905765656377, -7.653668647301794969 ) ) ;
#18360 = CARTESIAN_POINT ( 'NONE',  ( -28.68588794268869790, 256.3698905683720000, 16.75240474999999307 ) ) ;
#18361 = ORIENTED_EDGE ( 'NONE', *, *, #646, .F. ) ;
#18362 = CARTESIAN_POINT ( 'NONE',  ( -11.73070664223724613, 336.0573905765656377, 11.32908994701042005 ) ) ;
#18363 = CARTESIAN_POINT ( 'NONE',  ( -16.84014894278197616, 269.1198905683720568, 11.84573899990672530 ) ) ;
#18364 = CARTESIAN_POINT ( 'NONE',  ( -44.16309181155855867, 234.7448905683720000, -6.410867750099231266 ) ) ;
#18365 = CARTESIAN_POINT ( 'NONE',  ( -48.68588794268869435, 242.3073905765656377, 3.978247347593168115 ) ) ;
#18366 = CARTESIAN_POINT ( 'NONE',  ( 91.21585410611801592, 56.85652257517428865, -94.99999999999994316 ) ) ;
#18367 = CARTESIAN_POINT ( 'NONE',  ( -48.68588794268869435, 227.5573905601784759, 3.978247347593168115 ) ) ;
#18368 = VECTOR ( 'NONE', #15799, 1000.000000000000114 ) ;
#18369 = CARTESIAN_POINT ( 'NONE',  ( -11.93348319268871016, 268.8698905683720000, -2.051577885510841163E-15 ) ) ;
#18370 = VECTOR ( 'NONE', #21062, 1000.000000000000000 ) ;
#18371 = CARTESIAN_POINT ( 'NONE',  ( -45.43829269268870519, 355.6823905683720000, 3.332260488124734632 ) ) ;
#18372 = CARTESIAN_POINT ( 'NONE',  ( -45.64106924314017277, 278.1823905601785327, 11.32908994701042538 ) ) ;
#18373 = DIRECTION ( 'NONE',  ( 1.000000000000000000, 0.000000000000000000, -0.000000000000000000 ) ) ;
#18374 = CARTESIAN_POINT ( 'NONE',  ( -19.19641293061498999, 410.4323905683720568, -14.20200298773971603 ) ) ;
#18375 = CARTESIAN_POINT ( 'NONE',  ( -28.68588794268872633, 230.8848358243226073, 40.00000000000000000 ) ) ;
#18376 = ORIENTED_EDGE ( 'NONE', *, *, #13546, .F. ) ;
#18377 = CARTESIAN_POINT ( 'NONE',  ( -40.01497788969913927, 398.8073905601784759, 16.95518130045146776 ) ) ;
#18378 = ORIENTED_EDGE ( 'NONE', *, *, #8244, .F. ) ;
#18379 = ORIENTED_EDGE ( 'NONE', *, *, #17938, .F. ) ;
#18380 = EDGE_LOOP ( 'NONE', ( #20417, #3145 ) ) ;
#18381 = CARTESIAN_POINT ( 'NONE',  ( -11.93348319268874214, 530.6823905683721705, -3.332260488124732856 ) ) ;
#18382 = CARTESIAN_POINT ( 'NONE',  ( -32.66413529028186957, 295.0573905601784759, -19.99999999999999289 ) ) ;
#18383 = CARTESIAN_POINT ( 'NONE',  ( -43.15150032496258348, 208.1972798037766950, -3.972578417695637576 ) ) ;
#18384 = VECTOR ( 'NONE', #15676, 1000.000000000000000 ) ;
#18385 = CARTESIAN_POINT ( 'NONE',  ( -19.19641293061497578, 328.8073905683720568, 14.20200298773971426 ) ) ;
#18386 = ORIENTED_EDGE ( 'NONE', *, *, #18276, .F. ) ;
#18387 = CARTESIAN_POINT ( 'NONE',  ( -14.48388495494899786, 357.9323905683720568, 9.489475012073732785 ) ) ;
#18388 = CARTESIAN_POINT ( 'NONE',  ( -13.20868407381886023, 359.4948905683720000, -6.410867750099233042 ) ) ;
#18389 = CARTESIAN_POINT ( 'NONE',  ( -14.54375231895775933, 295.7448905765656377, 14.14213562373094568 ) ) ;
#18390 = PLANE ( 'NONE',  #4122 ) ;
#18391 = EDGE_CURVE ( 'NONE', #2137, #14411, #3381, .T. ) ;
#18392 = CARTESIAN_POINT ( 'NONE',  ( -40.53162694259542320, 265.1198905683720568, 11.84573899990672885 ) ) ;
#18393 = CARTESIAN_POINT ( 'NONE',  ( 40.42502041961814996, 170.1716627696692683, 40.00000000000000000 ) ) ;
#18394 = VECTOR ( 'NONE', #5999, 1000.000000000000000 ) ;
#18395 = CARTESIAN_POINT ( 'NONE',  ( -44.16309181155857999, 414.7448905683720568, -6.410867750099231266 ) ) ;
#18396 = CARTESIAN_POINT ( 'NONE',  ( -31.43424221336877622, 49.78331734519973395, 120.9832659038790865 ) ) ;
#18397 = CARTESIAN_POINT ( 'NONE',  ( -8.685887942688738761, 512.2448905601784190, -2.449293598294705724E-15 ) ) ;
#18398 = CARTESIAN_POINT ( 'NONE',  ( -45.64106924314017988, 358.1823905601784190, 11.32908994701042538 ) ) ;
#18399 = DIRECTION ( 'NONE',  ( -1.191790137725560488E-16, 1.000000000000000000, -0.000000000000000000 ) ) ;
#18400 = CARTESIAN_POINT ( 'NONE',  ( -19.19641293061497933, 328.8073905683720568, 14.20200298773971426 ) ) ;
#18401 = CARTESIAN_POINT ( 'NONE',  ( -11.93348319268873681, 489.1823905683720568, -3.332260488124732856 ) ) ;
#18402 = ORIENTED_EDGE ( 'NONE', *, *, #14073, .T. ) ;
#18403 = CARTESIAN_POINT ( 'NONE',  ( -42.82802356641967378, 465.9948905601784759, -14.14213562373094746 ) ) ;
#18404 = CARTESIAN_POINT ( 'NONE',  ( -25.35362745456398414, 301.0573905683720568, -16.75240474999999307 ) ) ;
#18405 = CARTESIAN_POINT ( 'NONE',  ( 32.47532367400565079, 585.7448905601785327, -163.9643442751439864 ) ) ;
#18406 = ORIENTED_EDGE ( 'NONE', *, *, #13147, .F. ) ;
#18407 = CARTESIAN_POINT ( 'NONE',  ( 20.42502041961814641, 160.1716627696692683, 40.00000000000000000 ) ) ;
#18408 = AXIS2_PLACEMENT_3D ( 'NONE', #2183, #3899, #15386 ) ;
#18409 = EDGE_CURVE ( 'NONE', #8588, #6213, #7115, .T. ) ;
#18410 = CARTESIAN_POINT ( 'NONE',  ( -28.68588794268871922, 382.8698905683720000, -16.75240474999999307 ) ) ;
#18411 = CARTESIAN_POINT ( 'NONE',  ( -48.68588794268871567, 441.9948905765656377, 0.000000000000000000 ) ) ;
#18412 = FACE_OUTER_BOUND ( 'NONE', #2187, .T. ) ;
#18413 = CARTESIAN_POINT ( 'NONE',  ( -45.43829269268871229, 433.5573905683719431, -3.332260488124726194 ) ) ;
#18414 = CARTESIAN_POINT ( 'NONE',  ( -35.09675569278793006, 253.4948905683720568, -15.47720386886985544 ) ) ;
#18415 = CARTESIAN_POINT ( 'NONE',  ( -22.27502019258949417, 430.7448905683720000, -15.47720386886985544 ) ) ;
#18416 = PRODUCT_CONTEXT ( 'NONE', #14281, 'mechanical' ) ;
#18417 =( BOUNDED_CURVE ( )  B_SPLINE_CURVE ( 2, ( #10064, #8334, #16578, #1542, #14746, #13436, #13002, #4992, #6496, #1655, #6820, #11589, #14957, #29, #1765, #143, #6717 ),
 .UNSPECIFIED., .F., .T. ) 
 B_SPLINE_CURVE_WITH_KNOTS ( ( 3, 2, 2, 2, 2, 2, 2, 2, 3 ),
 ( 0.1093750000000004580, 0.1113281250000004163, 0.1132812500000003747, 0.1152343750000003331, 0.1171875000000002776, 0.1191406250000002359, 0.1210937500000001943, 0.1230468750000001527, 0.1250000000000001110 ),
 .UNSPECIFIED. ) 
 CURVE ( )  GEOMETRIC_REPRESENTATION_ITEM ( )  RATIONAL_B_SPLINE_CURVE ( ( 0.9999999999999954481, 0.9807852804032349825, 1.000000000000000000, 0.9807852804032304306, 1.000000000000000000, 0.9807852804032304306, 1.000000000000000000, 0.9807852804032304306, 1.000000000000000000, 0.9807852804032304306, 1.000000000000000000, 0.9807852804032304306, 1.000000000000000000, 0.9807852804032304306, 1.000000000000000000, 0.9807852804032293204, 1.000000000000001110 ) ) 
 REPRESENTATION_ITEM ( '' )  );
#18418 = CARTESIAN_POINT ( 'NONE',  ( -42.82802356641966668, 398.4948905601784759, 14.14213562373094923 ) ) ;
#18419 = CARTESIAN_POINT ( 'NONE',  ( -24.70764059509555111, 354.8073905765655809, 19.99999999999998934 ) ) ;
#18420 = CARTESIAN_POINT ( 'NONE',  ( -45.64106924314017277, 276.3073905601784759, -11.32908994701042538 ) ) ;
#18421 = FACE_OUTER_BOUND ( 'NONE', #4481, .T. ) ;
#18422 = CARTESIAN_POINT ( 'NONE',  ( -42.88789093042843348, 334.8073905683720000, 9.489475012073734561 ) ) ;
#18423 = CARTESIAN_POINT ( 'NONE',  ( -49.57497958038185715, 160.1716627696692683, 60.00000000000000000 ) ) ;
#18424 = CARTESIAN_POINT ( 'NONE',  ( -45.43829269268872650, 475.3698905683720568, 0.000000000000000000 ) ) ;
#18425 = VECTOR ( 'NONE', #4834, 1000.000000000000000 ) ;
#18426 = DIRECTION ( 'NONE',  ( -1.000000000000000000, 1.854788578061058554E-16, 0.000000000000000000 ) ) ;
#18427 = LINE ( 'NONE', #13465, #13522 ) ;
#18428 = CARTESIAN_POINT ( 'NONE',  ( -42.91714575264039411, 206.7622684196151965, 4.742258924317273916 ) ) ;
#18429 = AXIS2_PLACEMENT_3D ( 'NONE', #3162, #3475, #25 ) ;
#18430 = ADVANCED_FACE ( 'NONE', ( #8337 ), #18180, .T. ) ;
#18431 = CARTESIAN_POINT ( 'NONE',  ( -11.93348319268872437, 390.6823905683720568, -3.332260488124732856 ) ) ;
#18432 = CARTESIAN_POINT ( 'NONE',  ( -45.64106924314019409, 471.0573905765656377, -11.32908994701042538 ) ) ;
#18433 = CARTESIAN_POINT ( 'NONE',  ( -47.16347859291446554, 526.6198905601784190, -7.653668647301793193 ) ) ;
#18434 = CARTESIAN_POINT ( 'NONE',  ( -16.84014894278198682, 367.6198905683720000, 11.84573899990672530 ) ) ;
#18435 = ORIENTED_EDGE ( 'NONE', *, *, #11471, .T. ) ;
#18436 = CARTESIAN_POINT ( 'NONE',  ( -28.68588794268873698, 531.3698905683720568, -16.75240474999999307 ) ) ;
#18437 = ORIENTED_EDGE ( 'NONE', *, *, #15151, .F. ) ;
#18438 = CARTESIAN_POINT ( 'NONE',  ( -38.17536295476245556, 436.9323905683720000, 14.20200298773971781 ) ) ;
#18439 = CARTESIAN_POINT ( 'NONE',  ( -11.93348319268874214, 528.8698905683719431, -2.051577885510841163E-15 ) ) ;
#18440 = EDGE_CURVE ( 'NONE', #21369, #7041, #19335, .T. ) ;
#18441 = VERTEX_POINT ( 'NONE', #11700 ) ;
#18442 = CARTESIAN_POINT ( 'NONE',  ( -40.01497788969915348, 495.6823905601784759, -16.95518130045146421 ) ) ;
#18443 = CARTESIAN_POINT ( 'NONE',  ( -14.48388495494901385, 487.9323905683719431, 9.489475012073732785 ) ) ;
#18444 = EDGE_LOOP ( 'NONE', ( #16066, #4401, #14963, #8263, #3278, #17410 ) ) ;
#18445 = CARTESIAN_POINT ( 'NONE',  ( -44.16309181155858710, 493.2448905683720000, -6.410867750099231266 ) ) ;
#18446 = CARTESIAN_POINT ( 'NONE',  ( -27.08348527696885810, 46.34737952406209160, -49.57559712733488055 ) ) ;
#18447 = AXIS2_PLACEMENT_3D ( 'NONE', #7008, #1957, #16667 ) ;
#18448 = CARTESIAN_POINT ( 'NONE',  ( -14.54375231895777532, 425.7448905765656377, 14.14213562373094568 ) ) ;
#18449 = FACE_OUTER_BOUND ( 'NONE', #17276, .T. ) ;
#18450 = LINE ( 'NONE', #3635, #6450 ) ;
#18451 = CARTESIAN_POINT ( 'NONE',  ( -45.64106924314018698, 441.0573905765656946, -11.32908994701042538 ) ) ;
#18452 = CARTESIAN_POINT ( 'NONE',  ( -28.68588794268875475, 600.7448905601785327, 0.000000000000000000 ) ) ;
#18453 = CARTESIAN_POINT ( 'NONE',  ( -42.83951137863823533, 204.4886979175576016, -4.967857365464206865 ) ) ;
#18454 = CARTESIAN_POINT ( 'NONE',  ( -45.43829269268869808, 305.0573905683720000, -3.332260488124726194 ) ) ;
#18455 = PLANE ( 'NONE',  #14744 ) ;
#18456 = CARTESIAN_POINT ( 'NONE',  ( -32.01814843081345430, 447.5573905683720000, 16.75240474999999307 ) ) ;
#18457 = LINE ( 'NONE', #3646, #3696 ) ;
#18458 = CARTESIAN_POINT ( 'NONE',  ( -42.88789093042842637, 286.3073905683720000, 9.489475012073736337 ) ) ;
#18459 = VERTEX_POINT ( 'NONE', #10066 ) ;
#18460 = CARTESIAN_POINT ( 'NONE',  ( -28.68588794268870146, 269.7448905601784759, 19.99999999999999289 ) ) ;
#18461 = CARTESIAN_POINT ( 'NONE',  ( -42.88789093042844769, 494.4323905683719431, -9.489475012073734561 ) ) ;
#18462 = VERTEX_POINT ( 'NONE', #16689 ) ;
#18463 = CARTESIAN_POINT ( 'NONE',  ( -38.17536295476246977, 473.8073905683720000, -14.20200298773971426 ) ) ;
#18464 = CARTESIAN_POINT ( 'NONE',  ( -8.685887942688726326, 392.2448905601784759, -2.449293598294705724E-15 ) ) ;
#18465 = CARTESIAN_POINT ( 'NONE',  ( -42.88789093042841927, 254.8073905683720284, 9.489475012073736337 ) ) ;
#18466 = EDGE_CURVE ( 'NONE', #451, #7864, #6085, .T. ) ;
#18467 = ORIENTED_EDGE ( 'NONE', *, *, #14867, .F. ) ;
#18468 = DIRECTION ( 'NONE',  ( -0.000000000000000000, 0.000000000000000000, 1.000000000000000000 ) ) ;
#18469 = EDGE_CURVE ( 'NONE', #8588, #6162, #15070, .T. ) ;
#18470 = CARTESIAN_POINT ( 'NONE',  ( -35.09675569278793716, 247.2448905683720000, 15.47720386886985366 ) ) ;
#18471 = FACE_OUTER_BOUND ( 'NONE', #3459, .T. ) ;
#18472 = PRODUCT_DEFINITION ( 'UNKNOWN', '', #11068, #2288 ) ;
#18473 = CARTESIAN_POINT ( 'NONE',  ( -32.66413529028186247, 229.4323905601785043, 19.99999999999999289 ) ) ;
#18474 = CARTESIAN_POINT ( 'NONE',  ( -38.17536295476244135, 275.4323905683720568, 14.20200298773971781 ) ) ;
#18475 = CARTESIAN_POINT ( 'NONE',  ( -45.43829269268870519, 355.0573905683720568, -3.332260488124726194 ) ) ;
#18476 = EDGE_CURVE ( 'NONE', #5103, #983, #466, .T. ) ;
#18477 = CARTESIAN_POINT ( 'NONE',  ( -45.64106924314019409, 506.3073905601784759, -11.32908994701042538 ) ) ;
#18478 = ADVANCED_FACE ( 'NONE', ( #7031 ), #7239, .T. ) ;
#18479 = CARTESIAN_POINT ( 'NONE',  ( 52.60622592008805043, 30.52886280891152282, 151.0302712373927250 ) ) ;
#18480 = VERTEX_POINT ( 'NONE', #13551 ) ;
#18481 = CARTESIAN_POINT ( 'NONE',  ( -48.68588794268871567, 397.2448905601784759, 0.000000000000000000 ) ) ;
#18482 = ORIENTED_EDGE ( 'NONE', *, *, #15061, .F. ) ;
#18483 = DIRECTION ( 'NONE',  ( 0.000000000000000000, 0.000000000000000000, 1.000000000000000000 ) ) ;
#18484 = ORIENTED_EDGE ( 'NONE', *, *, #13196, .F. ) ;
#18485 = ORIENTED_EDGE ( 'NONE', *, *, #14924, .F. ) ;
#18486 = CARTESIAN_POINT ( 'NONE',  ( -11.93348319268874036, 520.0573905683719431, 3.332260488124728415 ) ) ;
#18487 = CARTESIAN_POINT ( 'NONE',  ( -14.54375231895776110, 283.4948905601784759, -14.14213562373094746 ) ) ;
#18488 = CARTESIAN_POINT ( 'NONE',  ( 0.000000000000000000, 326.0737056351150613, 33.59072564020503648 ) ) ;
#18489 = CARTESIAN_POINT ( 'NONE',  ( -28.68588794268870856, 317.8698905683720000, 16.75240474999999307 ) ) ;
#18490 = ORIENTED_EDGE ( 'NONE', *, *, #113, .F. ) ;
#18491 = CARTESIAN_POINT ( 'NONE',  ( -28.68588794268871567, 371.3698905683720568, -16.75240474999999307 ) ) ;
#18492 = CARTESIAN_POINT ( 'NONE',  ( -28.68588794268871567, 371.3698905683720568, -16.75240474999999307 ) ) ;
#18493 = CARTESIAN_POINT ( 'NONE',  ( -40.01497788969913216, 310.4323905765656377, -16.95518130045146421 ) ) ;
#18494 = DIRECTION ( 'NONE',  ( 0.000000000000000000, 0.000000000000000000, 1.000000000000000000 ) ) ;
#18495 = CARTESIAN_POINT ( 'NONE',  ( -44.16309181155855157, 264.4948905683720000, 6.410867750099241924 ) ) ;
#18496 = CARTESIAN_POINT ( 'NONE',  ( -45.64106924314019409, 462.9323905765655809, 11.32908994701042538 ) ) ;
#18497 = CARTESIAN_POINT ( 'NONE',  ( -35.09675569278795138, 413.4948905683720000, -15.47720386886985544 ) ) ;
#18498 = PLANE ( 'NONE',  #12693 ) ;
#18499 = CARTESIAN_POINT ( 'NONE',  ( -11.73070664223726389, 506.0573905765656377, 11.32908994701042005 ) ) ;
#18500 = CARTESIAN_POINT ( 'NONE',  ( -11.73070664223723547, 276.0573905765655809, 11.32908994701042005 ) ) ;
#18501 = UNCERTAINTY_MEASURE_WITH_UNIT (LENGTH_MEASURE( 1.000000000000000082E-05 ), #9106, 'distance_accuracy_value', 'NONE');
#18502 = LINE ( 'NONE', #12014, #13938 ) ;
#18503 = CARTESIAN_POINT ( 'NONE',  ( -32.01814843081344009, 327.5573905683720568, 16.75240474999999307 ) ) ;
#18504 = CARTESIAN_POINT ( 'NONE',  ( -38.17536295476246977, 462.3073905683720568, -14.20200298773971426 ) ) ;
#18505 = ORIENTED_EDGE ( 'NONE', *, *, #15674, .T. ) ;
#18506 = CARTESIAN_POINT ( 'NONE',  ( -14.54375231895778420, 473.4948905601785327, -14.14213562373094746 ) ) ;
#18507 = CARTESIAN_POINT ( 'NONE',  ( -28.68588794268870501, 281.3698905683720000, -16.75240474999999307 ) ) ;
#18508 = ORIENTED_EDGE ( 'NONE', *, *, #18598, .F. ) ;
#18509 = DIRECTION ( 'NONE',  ( -2.775557561562891844E-16, 0.000000000000000000, -1.000000000000000000 ) ) ;
#18510 = ORIENTED_EDGE ( 'NONE', *, *, #248, .F. ) ;
#18511 = CARTESIAN_POINT ( 'NONE',  ( 0.000000000000000000, 0.000000000000000000, 0.000000000000000000 ) ) ;
#18512 = EDGE_CURVE ( 'NONE', #6728, #11704, #8870, .T. ) ;
#18513 = CARTESIAN_POINT ( 'NONE',  ( -44.16309181155857289, 384.7448905683720000, -6.410867750099231266 ) ) ;
#18514 = CIRCLE ( 'NONE', #19909, 9.999999999999980460 ) ;
#18515 = CARTESIAN_POINT ( 'NONE',  ( -28.68588794268874054, 573.2448905601785327, 0.000000000000000000 ) ) ;
#18516 = CARTESIAN_POINT ( 'NONE',  ( -24.70764059509555111, 384.8073905765655809, 19.99999999999998934 ) ) ;
#18517 = CARTESIAN_POINT ( 'NONE',  ( -14.48388495494900674, 429.8073905683720000, -9.489475012073736337 ) ) ;
#18518 = CARTESIAN_POINT ( 'NONE',  ( -38.17536295476243424, 266.9323905683720000, 14.20200298773971781 ) ) ;
#18519 = CARTESIAN_POINT ( 'NONE',  ( -14.48388495494900674, 419.8073905683720000, -9.489475012073734561 ) ) ;
#18520 = VECTOR ( 'NONE', #2584, 1000.000000000000000 ) ;
#18521 = CARTESIAN_POINT ( 'NONE',  ( -36.33955658999051508, 363.8698905765656377, 18.47759065022572500 ) ) ;
#18522 = CARTESIAN_POINT ( 'NONE',  ( -28.68588794268872277, 378.8848358243226357, 20.00000000000000000 ) ) ;
#18523 = CARTESIAN_POINT ( 'NONE',  ( -28.68588794268871212, 321.3698905683720568, -16.75240474999999307 ) ) ;
#18524 = CARTESIAN_POINT ( 'NONE',  ( -42.82802356641967378, 490.7448905765656377, -14.14213562373094746 ) ) ;
#18525 = CARTESIAN_POINT ( 'NONE',  ( -38.17536295476246977, 483.8073905683720000, -14.20200298773971426 ) ) ;
#18526 = DIRECTION ( 'NONE',  ( 0.000000000000000000, 0.000000000000000000, 1.000000000000000000 ) ) ;
#18527 = FACE_OUTER_BOUND ( 'NONE', #19164, .T. ) ;
#18528 = DIRECTION ( 'NONE',  ( 0.8666372666885295839, -0.4989387216749512355, 0.000000000000000000 ) ) ;
#18529 = EDGE_CURVE ( 'NONE', #13714, #3284, #18502, .T. ) ;
#18530 = VECTOR ( 'NONE', #15203, 1000.000000000000000 ) ;
#18531 = CARTESIAN_POINT ( 'NONE',  ( -38.17536295476245556, 396.9323905683721136, 14.20200298773971781 ) ) ;
#18532 = DIRECTION ( 'NONE',  ( 0.000000000000000000, 0.000000000000000000, 1.000000000000000000 ) ) ;
#18533 = CARTESIAN_POINT ( 'NONE',  ( -45.64106924314020119, 526.3073905601784190, -11.32908994701042715 ) ) ;
#18534 = CARTESIAN_POINT ( 'NONE',  ( -28.68588794268871212, 356.3698905683720568, 16.75240474999999307 ) ) ;
#18535 = AXIS2_PLACEMENT_3D ( 'NONE', #9350, #2980, #7928 ) ;
#18536 = ORIENTED_EDGE ( 'NONE', *, *, #2752, .F. ) ;
#18537 = ORIENTED_EDGE ( 'NONE', *, *, #4309, .T. ) ;
#18538 =( BOUNDED_CURVE ( )  B_SPLINE_CURVE ( 2, ( #8385, #1482, #6654, #6763, #6545, #18342, #21376, #16738, #10116, #13381, #18233, #14690, #16520, #3318, #19639, #14903, #21267 ),
 .UNSPECIFIED., .F., .T. ) 
 B_SPLINE_CURVE_WITH_KNOTS ( ( 3, 2, 2, 2, 2, 2, 2, 2, 3 ),
 ( 0.5312500000000003331, 0.5332031250000003331, 0.5351562500000003331, 0.5371093750000003331, 0.5390625000000003331, 0.5410156250000003331, 0.5429687500000003331, 0.5449218750000003331, 0.5468750000000003331 ),
 .UNSPECIFIED. ) 
 CURVE ( )  GEOMETRIC_REPRESENTATION_ITEM ( )  RATIONAL_B_SPLINE_CURVE ( ( 0.9999999999999966693, 0.9807852804032337612, 1.000000000000000000, 0.9807852804032304306, 1.000000000000000000, 0.9807852804032304306, 1.000000000000000000, 0.9807852804032304306, 1.000000000000000000, 0.9807852804032304306, 1.000000000000000000, 0.9807852804032304306, 1.000000000000000000, 0.9807852804032304306, 1.000000000000000000, 0.9807852804032270999, 1.000000000000003331 ) ) 
 REPRESENTATION_ITEM ( '' )  );
#18539 = CARTESIAN_POINT ( 'NONE',  ( -42.88789093042845479, 522.9323905683720568, -9.489475012073736337 ) ) ;
#18540 = ORIENTED_EDGE ( 'NONE', *, *, #8948, .F. ) ;
#18541 = CARTESIAN_POINT ( 'NONE',  ( -8.685887942688442109, 527.3073905765654672, -3.978247347592446914 ) ) ;
#18542 = CARTESIAN_POINT ( 'NONE',  ( -22.27502019258949062, 486.9948905683720568, 15.47720386886985189 ) ) ;
#18543 = ORIENTED_EDGE ( 'NONE', *, *, #10326, .F. ) ;
#18544 = CARTESIAN_POINT ( 'NONE',  ( -19.19641293061499354, 487.3073905683719431, 14.20200298773971426 ) ) ;
#18545 = CARTESIAN_POINT ( 'NONE',  ( -19.19910310533017750, 45.73968925459546142, -48.68588693060413419 ) ) ;
#18546 = EDGE_CURVE ( 'NONE', #15608, #19361, #16665, .T. ) ;
#18547 = AXIS2_PLACEMENT_3D ( 'NONE', #4054, #15219, #721 ) ;
#18548 = CARTESIAN_POINT ( 'NONE',  ( -10.20829729246299244, 416.3698905765656377, 7.653668647301790529 ) ) ;
#18549 = CARTESIAN_POINT ( 'NONE',  ( -45.64106924314019409, 472.9323905765655809, 11.32908994701042538 ) ) ;
#18550 = CARTESIAN_POINT ( 'NONE',  ( 51.50493485826542184, 170.1716627696692683, -20.00000000000000355 ) ) ;
#18551 = DIRECTION ( 'NONE',  ( 0.000000000000000000, 0.000000000000000000, -1.000000000000000000 ) ) ;
#18552 =( REPRESENTATION_RELATIONSHIP ('NONE','NONE', #1888, #15840 ) REPRESENTATION_RELATIONSHIP_WITH_TRANSFORMATION ( #7154 )SHAPE_REPRESENTATION_RELATIONSHIP( ) );
#18553 = DIRECTION ( 'NONE',  ( 1.191790137725560488E-16, -1.000000000000000000, -0.000000000000000000 ) ) ;
#18554 = AXIS2_PLACEMENT_3D ( 'NONE', #21327, #5096, #11698 ) ;
#18555 = CARTESIAN_POINT ( 'NONE',  ( -4.764560328305437435E-16, -0.6346842323199950453, -6.500000000000000000 ) ) ;
#18556 = CARTESIAN_POINT ( 'NONE',  ( 115.7989814974898337, 142.5259582928263455, -40.00000000000000000 ) ) ;
#18557 = CARTESIAN_POINT ( 'NONE',  ( -45.43829269268870519, 295.3698905683720568, 0.000000000000000000 ) ) ;
#18558 = EDGE_CURVE ( 'NONE', #13710, #683, #2194, .T. ) ;
#18559 = DIRECTION ( 'NONE',  ( -0.5877852522924731371, -7.005166667826997985E-17, 0.8090169943749475623 ) ) ;
#18560 = CARTESIAN_POINT ( 'NONE',  ( -42.88789093042844769, 456.3073905683720000, 9.489475012073736337 ) ) ;
#18561 = CARTESIAN_POINT ( 'NONE',  ( -33.23789986170869071, 53.12371016881039054, -49.39189772945173473 ) ) ;
#18562 = CARTESIAN_POINT ( 'NONE',  ( -11.93348319268871016, 270.3698905683720000, -2.051577885510841163E-15 ) ) ;
#18563 = VECTOR ( 'NONE', #3952, 1000.000000000000000 ) ;
#18564 = VERTEX_POINT ( 'NONE', #1981 ) ;
#18565 = CARTESIAN_POINT ( 'NONE',  ( -40.01497788969911795, 268.8073905601784759, 16.95518130045146776 ) ) ;
#18566 = CARTESIAN_POINT ( 'NONE',  ( -44.16309181155858710, 504.7448905683720000, -6.410867750099231266 ) ) ;
#18567 = AXIS2_PLACEMENT_3D ( 'NONE', #3663, #8740, #20001 ) ;
#18568 = ORIENTED_EDGE ( 'NONE', *, *, #18409, .T. ) ;
#18569 = CARTESIAN_POINT ( 'NONE',  ( -40.53162694259545162, 464.1198905683720568, -11.84573899990672707 ) ) ;
#18570 = LINE ( 'NONE', #1834, #11806 ) ;
#18571 = CARTESIAN_POINT ( 'NONE',  ( -44.16309181155855867, 263.2448905683720000, -6.410867750099231266 ) ) ;
#18572 = VERTEX_POINT ( 'NONE', #4001 ) ;
#18573 = CARTESIAN_POINT ( 'NONE',  ( -24.70764059509554755, 334.8073905765656946, 19.99999999999998934 ) ) ;
#18574 = CARTESIAN_POINT ( 'NONE',  ( 0.05533025579362052526, 4.993776679985852951, 4.350525068611870161 ) ) ;
#18575 = CARTESIAN_POINT ( 'NONE',  ( -40.53162694259542320, 236.6198905683720284, 11.84573899990672885 ) ) ;
#18576 = CARTESIAN_POINT ( 'NONE',  ( -40.01497788969912506, 308.8073905601784759, 16.95518130045146776 ) ) ;
#18577 = CARTESIAN_POINT ( 'NONE',  ( -11.73070664223723369, 233.1823905601784475, -11.32908994701042715 ) ) ;
#18578 = CARTESIAN_POINT ( 'NONE',  ( -22.27502019258947641, 270.7448905683720568, -15.47720386886985544 ) ) ;
#18579 = CARTESIAN_POINT ( 'NONE',  ( -44.16309181155856578, 365.9948905683720568, 6.410867750099241924 ) ) ;
#18580 = CARTESIAN_POINT ( 'NONE',  ( -42.88789093042844058, 404.8073905683721136, 9.489475012073736337 ) ) ;
#18581 = DIRECTION ( 'NONE',  ( -0.000000000000000000, -0.000000000000000000, -1.000000000000000000 ) ) ;
#18582 = CARTESIAN_POINT ( 'NONE',  ( -24.70764059509555821, 410.0573905601784759, 19.99999999999998934 ) ) ;
#18583 = CIRCLE ( 'NONE', #4783, 6.500000000000000888 ) ;
#18584 = ORIENTED_EDGE ( 'NONE', *, *, #10920, .F. ) ;
#18585 = DIRECTION ( 'NONE',  ( 0.000000000000000000, 0.000000000000000000, 1.000000000000000000 ) ) ;
#18586 = ORIENTED_EDGE ( 'NONE', *, *, #20375, .T. ) ;
#18587 = VERTEX_POINT ( 'NONE', #17110 ) ;
#18588 = CARTESIAN_POINT ( 'NONE',  ( -19.19641293061500420, 531.9323905683720568, -14.20200298773971603 ) ) ;
#18589 = CARTESIAN_POINT ( 'NONE',  ( -11.73070664223723547, 281.3073905601784759, 11.32908994701042005 ) ) ;
#18590 = CARTESIAN_POINT ( 'NONE',  ( -11.73070664223724613, 317.9323905765656377, -11.32908994701042538 ) ) ;
#18591 = EDGE_CURVE ( 'NONE', #20328, #2535, #3791, .T. ) ;
#18592 = CARTESIAN_POINT ( 'NONE',  ( -35.09675569278794427, 317.2448905683720000, 15.47720386886985366 ) ) ;
#18593 = ORIENTED_EDGE ( 'NONE', *, *, #15846, .F. ) ;
#18594 = CARTESIAN_POINT ( 'NONE',  ( -32.01814843081344719, 351.6823905683720000, -16.75240474999999307 ) ) ;
#18595 = ADVANCED_FACE ( 'NONE', ( #13653 ), #5520, .F. ) ;
#18596 = CARTESIAN_POINT ( 'NONE',  ( -35.09675569278795138, 365.7448905683720568, 15.47720386886985366 ) ) ;
#18597 = EDGE_CURVE ( 'NONE', #795, #20892, #19446, .T. ) ;
#18598 = EDGE_CURVE ( 'NONE', #5454, #9142, #5410, .T. ) ;
#18599 = CARTESIAN_POINT ( 'NONE',  ( -17.35679799567829207, 308.5573905765656377, -16.95518130045146421 ) ) ;
#18600 = CARTESIAN_POINT ( 'NONE',  ( 27.98965548446208373, 333.8848358243226357, -40.00000000000000000 ) ) ;
#18601 = CARTESIAN_POINT ( 'NONE',  ( -38.17536295476244845, 272.3073905683720000, -14.20200298773971426 ) ) ;
#18602 = CARTESIAN_POINT ( 'NONE',  ( -42.99843930773590017, 202.9216059526224569, 4.490902998358461851 ) ) ;
#18603 = CARTESIAN_POINT ( 'NONE',  ( -25.35362745456398770, 418.1823905683720568, 16.75240474999998952 ) ) ;
#18604 = DIRECTION ( 'NONE',  ( 0.000000000000000000, -1.000000000000000000, 0.000000000000000000 ) ) ;
#18605 = CARTESIAN_POINT ( 'NONE',  ( -14.54375231895778420, 505.7448905765655809, 14.14213562373094568 ) ) ;
#18606 = DIRECTION ( 'NONE',  ( -0.000000000000000000, -0.000000000000000000, -1.000000000000000000 ) ) ;
#18607 = EDGE_CURVE ( 'NONE', #1064, #1192, #20030, .T. ) ;
#18608 = CARTESIAN_POINT ( 'NONE',  ( -28.68588794268870856, 327.8698905683720000, 16.75240474999999307 ) ) ;
#18609 = CARTESIAN_POINT ( 'NONE',  ( -13.20868407381887089, 468.2448905683720568, 6.410867750099229490 ) ) ;
#18610 = ORIENTED_EDGE ( 'NONE', *, *, #11824, .F. ) ;
#18611 = CARTESIAN_POINT ( 'NONE',  ( -10.20829729246299955, 472.8698905601784759, -7.653668647301794969 ) ) ;
#18612 = CARTESIAN_POINT ( 'NONE',  ( -14.48388495494898720, 277.9323905683720000, 9.489475012073732785 ) ) ;
#18613 = ORIENTED_EDGE ( 'NONE', *, *, #15578, .F. ) ;
#18614 = LINE ( 'NONE', #3800, #12242 ) ;
#18615 = CARTESIAN_POINT ( 'NONE',  ( -36.33955658999051508, 339.1198905601784759, 18.47759065022572500 ) ) ;
#18616 = CARTESIAN_POINT ( 'NONE',  ( -45.43829269268869808, 303.5573905683720568, -3.332260488124726194 ) ) ;
#18617 = CIRCLE ( 'NONE', #6509, 4.000000000000001776 ) ;
#18618 = CARTESIAN_POINT ( 'NONE',  ( -16.84014894278199037, 379.1198905683720568, 11.84573899990672530 ) ) ;
#18619 = CARTESIAN_POINT ( 'NONE',  ( -73.08746600497821078, 600.7448905601785327, -22.98912494155474207 ) ) ;
#18620 = CARTESIAN_POINT ( 'NONE',  ( -32.01814843081345430, 396.0573905683720568, 16.75240474999999307 ) ) ;
#18621 = CARTESIAN_POINT ( 'NONE',  ( -45.43829269268869098, 265.0573905683720568, -3.332260488124726194 ) ) ;
#18622 = CARTESIAN_POINT ( 'NONE',  ( -42.88789093042844058, 434.8073905683721136, 9.489475012073734561 ) ) ;
#18623 = CONTEXT_DEPENDENT_SHAPE_REPRESENTATION ( #15946, #19781 ) ;
#18624 = CARTESIAN_POINT ( 'NONE',  ( -21.03221929538692336, 358.8698905765656377, -18.47759065022572855 ) ) ;
#18625 = DIRECTION ( 'NONE',  ( 1.191790137725560488E-16, -1.000000000000000000, 0.000000000000000000 ) ) ;
#18626 = CARTESIAN_POINT ( 'NONE',  ( -13.20868407381885312, 318.2448905683720000, 6.410867750099229490 ) ) ;
#18627 = CARTESIAN_POINT ( 'NONE',  ( -19.19641293061499709, 471.9323905683720568, -14.20200298773971603 ) ) ;
#18628 = CARTESIAN_POINT ( 'NONE',  ( -14.54375231895777532, 435.7448905765656377, 14.14213562373094568 ) ) ;
#18629 = CARTESIAN_POINT ( 'NONE',  ( -42.82802356641964536, 205.1437886375728965, -5.000000000000001776 ) ) ;
#18630 = CARTESIAN_POINT ( 'NONE',  ( -11.73070664223723014, 226.0573905765656093, 11.32908994701042005 ) ) ;
#18631 = AXIS2_PLACEMENT_3D ( 'NONE', #14820, #8084, #21291 ) ;
#18632 = CARTESIAN_POINT ( 'NONE',  ( -13.20868407381886200, 380.9948905683720568, -6.410867750099233042 ) ) ;
#18633 = CARTESIAN_POINT ( 'NONE',  ( -32.63738144191441393, 51.69676759036851621, -120.6641474517143422 ) ) ;
#18634 = CARTESIAN_POINT ( 'NONE',  ( -45.64106924314020119, 528.1823905601785327, 11.32908994701042715 ) ) ;
#18635 = CARTESIAN_POINT ( 'NONE',  ( -13.20868407381885667, 338.2448905683720568, 6.410867750099229490 ) ) ;
#18636 = ORIENTED_EDGE ( 'NONE', *, *, #10463, .T. ) ;
#18637 = CARTESIAN_POINT ( 'NONE',  ( -11.93348319268874214, 528.5573905683720568, 3.332260488124728415 ) ) ;
#18638 = ORIENTED_EDGE ( 'NONE', *, *, #1933, .T. ) ;
#18639 = CARTESIAN_POINT ( 'NONE',  ( -44.93162628806840786, 223.9102039777116602, -4.140855835305760735 ) ) ;
#18640 = CARTESIAN_POINT ( 'NONE',  ( -8.685887942688539809, 312.5573905601784190, -3.978247347592740013 ) ) ;
#18641 = DIRECTION ( 'NONE',  ( -1.000000000000000000, 0.000000000000000000, 0.000000000000000000 ) ) ;
#18642 = CARTESIAN_POINT ( 'NONE',  ( -48.68588794268872277, 497.2448905601785327, 0.000000000000000000 ) ) ;
#18643 = CARTESIAN_POINT ( 'NONE',  ( -11.93348319268873503, 478.8698905683720568, -2.051577885510841163E-15 ) ) ;
#18644 = ORIENTED_EDGE ( 'NONE', *, *, #10003, .T. ) ;
#18645 = CARTESIAN_POINT ( 'NONE',  ( -22.27502019258949773, 480.7448905683720568, -15.47720386886985544 ) ) ;
#18646 = CARTESIAN_POINT ( 'NONE',  ( -16.38242098736782992, 46.95008282854134052, -48.05128789156074021 ) ) ;
#18647 = EDGE_CURVE ( 'NONE', #10685, #19682, #815, .T. ) ;
#18648 = CARTESIAN_POINT ( 'NONE',  ( -42.82802356641966668, 420.7448905765656377, -14.14213562373094746 ) ) ;
#18649 = CARTESIAN_POINT ( 'NONE',  ( 28.16023193154655502, 323.8848358243226357, -40.00000000000000000 ) ) ;
#18650 = CARTESIAN_POINT ( 'NONE',  ( 60.03793209889851568, 30.52886280891152282, 131.1729372809869005 ) ) ;
#18651 = DIRECTION ( 'NONE',  ( -0.000000000000000000, -0.000000000000000000, -1.000000000000000000 ) ) ;
#18652 = DIRECTION ( 'NONE',  ( -1.191790137725560488E-16, 1.000000000000000000, 0.000000000000000000 ) ) ;
#18653 = DIRECTION ( 'NONE',  ( 0.000000000000000000, 0.000000000000000000, 1.000000000000000000 ) ) ;
#18654 = FACE_BOUND ( 'NONE', #12753, .T. ) ;
#18655 = ADVANCED_FACE ( 'NONE', ( #15488 ), #4597, .T. ) ;
#18656 = CARTESIAN_POINT ( 'NONE',  ( 35.96497763894179656, 191.2380552923725645, 48.74187950074039577 ) ) ;
#18657 = CARTESIAN_POINT ( 'NONE',  ( -32.01814843081344009, 287.5573905683719431, 16.75240474999999307 ) ) ;
#18658 = DIRECTION ( 'NONE',  ( 0.000000000000000000, 0.000000000000000000, -1.000000000000000000 ) ) ;
#18659 = CARTESIAN_POINT ( 'NONE',  ( -13.20868407381886911, 449.7448905683720000, 6.410867750099229490 ) ) ;
#18660 = FACE_OUTER_BOUND ( 'NONE', #6829, .T. ) ;
#18661 =( BOUNDED_SURFACE ( )  B_SPLINE_SURFACE ( 1, 2, ( 
 ( #16988, #6909, #10159, #3675, #8429, #7014, #343, #5082, #6804, #235, #10471, #18588, #10257, #14942, #13422, #18381, #20012, #16879, #5501, #15053, #11683, #1859, #7119, #3462, #20121, #447, #2168, #13744, #1963, #3570, #5189, #8751, #127, #13318, #13532, #18273, #15372, #550, #19901, #20330, #16778, #10049, #5290, #16673, #11786, #2062, #8534, #15158, #11893, #18486, #12103, #8638, #15265, #13637, #3883, #20223, #5392, #18695, #17092, #9068, #20548, #13963, #5714, #4318, #12546, #9172, #5611, #9284, #7440, #11008, #14066, #2703, #14287, #12219, #18803, #15473, #12322, #6039, #18910, #15689, #10901, #4095, #12649, #10683, #17301, #15900, #875, #17199, #17511, #3985, #19241, #4424, #2485, #8960, #2273, #8852, #10576, #7659, #20651, #20437, #767, #15583, #658, #19140, #19026, #7223, #7332, #5821, #12431, #4212, #20873, #10795, #2378, #17411, #1091, #2593, #15798, #985, #13844, #7549, #14174, #20763, #5932, #13072, #17617, #9393, #1395, #20975, #19656, #11436, #16012, #9808, #12860, #1194, #7970, #7764, #14391, #12963, #2809, #11227, #11117, #6143, #1609, #14600, #11330, #12754, #13182, #4633, #19344, #2917, #19450, #3017, #14494, #7865, #21075, #4836, #6456, #3122, #4530, #3232, #21182, #4952, #6353, #18036, #8182, #17720, #9497, #16110, #6249, #16280, #17824, #9600, #16430, #16218, #6561, #19553, #4734, #14812, #17925, #1289, #19766, #9707, #16326, #1502, #8076, #14706, #21283, #18141, #14919, #16963, #9917, #10025, #19986, #8404, #15029, #6674, #6993, #18463, #3652, #13715, #11657, #20202, #10234, #16536, #13615, #3441, #3335, #16859, #5268, #20308, #5367, #102, #16651, #6780, #8612, #6886, #7096, #13293, #10339, #318, #11972, #10135, #13400, #13506, #18249, #2041, #18358, #5055, #18569, #19878, #11551, #1721, #213, #1833, #531, #8293, #5167, #2142, #11763, #3549, #16755, #1942, #8510, #15137, #3751, #15236, #427, #20099, #11873, #8723, #15350, #3645, #7301, #18560, #11861, #12184, #20404, #5262, #13927, #15226, #3743, #524, #2346, #626, #842, #419, #4066, #15439, #734, #3851, #7085, #7191, #5360, #3958, #18659, #2035, #10330, #16952, #7408, #15550, #13814, #18456, #2134, #15340, #8715, #5579, #2453, #11963, #8603, #20191, #10650, #6985, #17061, #18770, #20515, #17270, #20299, #13707, #5471, #5684, #10227, #16850, #10440, #13606, #12290, #18876, #12069, #9034, #2244, #8822, #10546, #17167, #8926, #15657, #5790, #14249, #14139, #20615, #4598, #4389, #14357, #15760, #16182, #7621, #949, #5899, #15867, #6006, #17474, #10868, #2662, #1253, #9463, #6107, #2557, #6209, #10973, #7931, #17582, #21041, #11191, #9139, #7515, #12396, #9250, #2983, #1056, #12615, #7831, #20835, #9564, #19206, #2774, #12825, #12719, #20937, #18988, #14459, #20725, #12509, #9357, #17687, #15974, #1359, #19102, #19414, #1158, #16075, #7729, #19308, #4494, #4286, #11080, #2879, #17376, #17791, #4169, #10760, #3407, #9880, #21147, #6417, #3195, #19624, #16503, #11729, #21252, #11295, #8041, #13363, #9667, #4915, #6636, #9986, #19954, #8143, #9773, #4802, #16610, #14562, #6319, #19733, #17891, #1800, #8367, #12933, #6746, #16398, #19519, #11513, #4698, #3085, #1683, #16293, #14774, #14674, #1466, #5131, #18107, #8255, #13034, #10097, #1575, #11398, #18000, #21359, #6527, #13143, #3303, #14884, #14992, #177, #69, #13257, #18321, #19844, #1908, #5020, #3510, #16719, #11621, #18216, #283, #18531, #12262, #20170, #497, #17138, #3718, #18844, #5336, #11936, #15517, #15310, #2012, #2319, #11834, #4034, #10624, #10302, #15202, #17241, #15098, #18431, #13896, #6851, #6957, #16928, #2109, #8689, #3616, #3930, #15413, #597, #8475, #8579, #8899, #7162, #13470, #10515, #391, #20060, #5235, #10201, #3821, #16822, #7060, #13580, #13679, #20485, #20270, #2212, #5442, #12041, #18632, #10411, #17032, #8796, #13785, #20373, #5547, #12154, #702, #18741, #7271, #5657, #9434, #7590, #11162, #14219, #2852, #14434, #5757, #12367, #15627, #12479, #6184, #14110, #15838, #11048, #19072, #12795, #20695, #5868, #16053, #9219, #17345, #17660, #18955, #19387, #4572, #4255, #9112, #2424, #9006, #4138, #7802, #813, #920, #10842, #17447, #1025, #10731, #19282, #9324, #15943, #14007, #2529, #1230, #1130, #20587, #4465, #15733, #7483, #7702, #17554, #20807, #5976, #12588, #19180, #4357, #20910, #10944, #2743, #14330, #6076, #12689, #13229, #16369, #19598, #13116, #17864, #16476, #9748, #14533, #16262, #9642, #19922, #6607, #19701, #2957, #1440, #6393, #8011, #4886, #14961, #3057, #21118, #11265, #16581, #12904, #8117, #9849, #19819, #1769, #11371, #13004, #14644, #4995, #17765, #9534, #1545, #6290, #11594, #18185, #16154, #9962, #4774, #1332, #14749, #21332, #8228, #1659, #13338, #33, #21228, #3383, #6499, #18081, #7905, #17966, #8338, #148, #3169, #6721, #5101, #19495, #4673, #11484, #14857, #3275, #10067, #13552, #1983, #6928, #13654, #8659, #20141, #2080, #5411, #18294, #8769, #675, #18712, #7240, #20347, #12124, #11702, #3691, #5207, #362, #5522, #10279, #7032, #5308, #15284, #20239, #12015, #3588, #13761, #467, #18400, #11909, #8447, #18608, #18503, #3900, #3481, #10489, #3792, #15387, #15174, #2290, #11804, #567, #7135, #8871, #16690, #1879, #16898, #10384, #15489, #17004, #8554, #17111, #15072, #13868, #2185, #20456, #256, #16795, #6823, #13439, #10174, #4727, #19547, #9386, #9699, #8977, #7652, #8070, #1388, #11110, #2799, #1280, #2911, #19442, #4002, #6030, #16004, #21175, #14487, #15601, #16320, #4521, #1081, #12237, #10594, #14593, #1495, #14278, #17713, #5627, #9594, #6347, #2395, #11325, #9491, #17919, #12744, #14700, #18820, #3117, #16211, #12642, #21067, #7859, #17608, #17214, #20865, #1187, #19233, #16103, #4416, #10999, #6240, #7756, #20966, #14383, #6136, #19336, #12853, #4627, #11221, #17818, #3010, #7961, #12958, #1716, #6668, #18135, #11545, #3328, #1937, #10128, #6773, #3224, #6880, #5049, #8605, #11650, #312, #11863, #9802, #16424, #13065, #9910, #3647, #8283, #13289, #8503, #14913, #10229, #19873, #18244, #13500, #3436, #14807, #15129, #1602, #16851, #21277, #10018, #6556, #6449, #19651, #8176, #18458, #4831, #19762, #16642, #1828, #8397, #21390, #16750, #13394, #19981, #11429, #13176, #20093, #5161, #18031, #4945, #15024, #207, #11757, #3541, #2559, #2455, #3745, #7087, #10442, #12292, #10548, #10762, #10332, #14035, #3960, #10652, #13816, #17063, #17170, #15342, #13929, #7193, #11965, #13709, #20301, #17378, #4068, #2348, #421, #5473, #3853, #12071, #8928, #12398, #526, #18562, #8718, #20617, #16954, #5581, #7303, #17272, #5792, #8824, #2246, #18662, #9036, #15228, #6987, #20406, #2136, #15658, #844, #7409, #13608, #20194, #12186, #15441, #18990, #4172, #5362, #628, #18772, #15552, #736, #20517, #5686, #18878, #15762, #2776, #2664, #9141, #14564, #14359, #2881, #4288, #4701, #17584, #10870, #15869, #4391, #15976, #6008, #20837, #12618, #11193, #19416, #16077, #12511, #16184, #20939, #17893, #6109, #9567, #21149, #19104, #17476, #951, #19208, #12934, #10975, #1160, #17793, #9360, #19521, #7731, #12721, #1361, #19310, #9252, #2985, #1057, #11297, #7517, #4496, #7624, #14141, #20727, #14251, #6321, #5901, #11084, #17689, #9465, #1255, #7833, #4600, #14461, #21043, #6211, #12827, #7934, #9988, #1468, #5133, #16400, #9670, #16612, #18218, #11837, #11732, #13036, #1577, #19735, #180, #19846, #20064, #19626, #1910, #13260, #19956, #1685, #4919, #5023, #3197, #1802, #16506, #21254, #8146, #14776, #5237, #13365, #11623, #16295, #21361, #13146, #6530, #3409, #285, #9775, #6419, #18003, #8478, #4804, #14886, #8370, #18323, #15100, #18109, #11516, #3305, #16721, #8257, #6853, #9882, #3087, #13472, #8044, #6748, #71, #14994, #3513, #6639, #10100 ),
 ( #11400, #14676, #10203, #7062, #816, #8691, #10413, #5659, #13681, #7383, #15314, #500, #4036, #3825, #11938, #12264, #394, #14009, #20589, #20272, #3721, #5759, #3618, #6960, #2426, #16825, #16930, #5444, #12044, #18634, #13583, #13898, #3932, #10518, #18433, #18533, #18848, #17140, #2014, #20488, #10304, #8581, #2321, #12156, #15204, #10626, #20172, #2112, #17034, #15519, #13787, #5338, #2215, #17243, #7164, #9008, #8798, #15415, #20377, #599, #8901, #5550, #18744, #704, #7275, #15631, #1232, #7705, #18957, #4257, #1027, #17449, #14333, #9536, #19074, #9114, #5870, #11165, #7486, #2745, #4469, #7804, #17767, #5980, #7592, #2636, #14436, #12369, #14112, #4140, #17348, #21017, #7907, #15735, #10946, #10734, #16055, #6186, #921, #4574, #17556, #2959, #19183, #21121, #16156, #1334, #12798, #10845, #20912, #6078, #9221, #9326, #2854, #11050, #14535, #19389, #12482, #2531, #1132, #12691, #20697, #15841, #14222, #20809, #12590, #4360, #15947, #19284, #17662, #9437, #18188, #19497, #4675, #8120, #17969, #1548, #8231, #3279, #14752, #18085, #36, #12907, #3386, #16693, #13341, #1882, #14964, #6724, #6292, #19704, #21230, #16374, #152, #4890, #1662, #21335, #9852, #14860, #6611, #19600, #8342, #16479, #13006, #6503, #3059, #13232, #13119, #19926, #11267, #5104, #19823, #9965, #9751, #18297, #14647, #16584, #1772, #3484, #17866, #9644, #11487, #4998, #10072, #11599, #3172, #11705, #16264, #8450, #15075, #1443, #8014, #11373, #6395, #4776, #15390, #20460, #13871, #3694, #4005, #3591, #1986, #2398, #17114, #5414, #18506, #17008, #18611, #13764, #20034, #365, #10282, #15492, #8772, #10177, #10597, #20242, #678, #13657, #2188, #8662, #3795, #570, #7138, #13556, #2293, #10387, #6931, #16901, #18403, #20350, #470, #7243, #13442, #5630, #5525, #18716, #2083, #12240, #8557, #3903, #8874, #18823, #5210, #6827, #7035, #12127, #17217, #10492, #11912, #8980, #11809, #259, #15287, #12018, #16798, #5311, #15178, #20144, #9303, #14412, #7780, #19048, #19363, #18930, #17321, #17741, #11025, #20784, #12449, #10919, #12566, #7679, #13982, #15707, #4233, #9413, #2722, #4114, #4550, #14193, #10702, #791, #20565, #2828, #11138, #2505, #5951, #15604, #19259, #16029, #12343, #20994, #19161, #6159, #1003, #2933, #7351, #12772, #4441, #894, #15917, #17530, #5843, #4338, #6056, #14305, #5733, #17636, #7458, #1210, #1108, #20889, #9088, #20669, #14087, #10815, #17429, #2610, #9193, #15818, #7567, #12667, #10, #1312, #7884, #11349, #21206, #4753, #11456, #6476, #17945, #21305, #3250, #16130, #6584, #19897, #16557, #5076, #18159, #9936, #9513, #1522, #3037, #19572, #19678, #9826, #14511, #14621, #3358, #19789, #3142, #11570, #1741, #21095, #8314, #6267, #13205, #12883, #19470, #9724, #6371, #16347, #18056, #13092, #8095, #4861, #16450, #4653, #4972, #11678, #14937, #18268, #121, #6695, #11243, #14724, #9620, #1632, #13313, #8205, #14833, #17841, #16239, #1416, #7990, #12981, #5496, #442, #10155, #20116, #231, #3770, #3668, #10466, #16669, #18690, #5386, #545, #6904, #15468, #11782, #7114, #20324, #652, #1855, #10044, #10252, #18582, #7217, #10357, #15155, #13739, #8424, #13839, #11888, #15260, #7009, #8529, #13632, #15367, #16982, #2268, #17087, #13527, #20432, #6800, #5185, #5606, #12098, #8632, #337, #20218, #11992, #2163, #15048, #3566, #5285, #3877, #8746, #13417, #12212, #2058, #20008, #18377, #16772, #8846, #3458, #1959, #18481, #16874, #1087, #12645, #15577, #11002, #17406, #9389, #4207, #6139, #1190, #17613, #7655, #4090, #5927, #14169, #9063, #9167, #9279, #17505, #14387, #14283, #18906, #20869, #10678, #2698, #10789, #762, #17297, #2480, #20970, #6034, #20758, #3981, #15684, #7434, #870, #12541, #16008, #14061, #7327, #12317, #2805, #13958, #15791, #10896, #19236, #7760, #12425, #20646, #5816, #4420, #18798, #10570, #2588, #20542, #17194, #2372, #8955, #5709, #19022, #980, #7543, #19134, #4313, #15896, #19339, #6350, #6245, #12749, #18137, #17921, #6452, #7862, #8288, #21179, #14490, #19447, #7967, #19550, #9597, #3013, #16214, #14809, #1605, #19653, #16107, #19764, #3119, #99, #9703, #13179, #3331, #1285, #21072, #4527, #1391, #16533, #14596, #4730, #20423, #12960, #1718, #11327, #16323, #4949, #1498, #12857, #6558, #4630, #14916, #11114, #8073, #11224, #17717, #2914, #17821, #9913, #9494, #14703, #21279, #13068, #4833, #11433, #8178, #18033, #3229, #9804, #16427, #11548, #13903, #11944, #821, #12050, #13588, #20493, #12269, #15740, #5766, #2117, #10418, #2221, #10631, #15526, #10310, #8696, #18964, #4145, #7067, #5555, #8803, #7170, #12162, #20382, #18749, #18937, #20571, #10182, #4012, #16907, #18721, #5530, #477, #575, #7251, #8881, #16803, #10606, #10287, #17224, #20355, #10500, #1992, #15292, #2406, #8562, #5422, #15183, #369, #5317, #2088, #8668, #7043, #13662, #20249, #12023, #18615, #3801, #12134, #7144, #10393, #13768, #3909, #17012, #8778, #15499, #11142, #21100, #12777, #4555, #4120, #17536, #19054, #14201, #19370, #2728, #20894, #12571, #7684, #12672, #19265, #17434, #6164, #1114, #10823, #20790, #900, #4446, #4344, #17747, #17328, #2938, #6062, #1215, #7573, #16135, #12455, #7785, #20999, #1318, #2511, #10708, #10925, #11031, #7889, #17641, #15824, #14417, #9095, #14516, #19166, #15922, #14311, #9198, #2834, #16034, #9417, #9518, #6273, #5956, #12888, #7464, #5850, #15714, #14094, #9307, #1009, #20675, #4238, #2616, #17846, #19577, #8099, #13319, #6589, #7994, #1860, #18061, #14627, #4658, #3042, #6700, #15054, #1420, #3256, #19476, #1747, #19902, #16244, #11684, #16563, #1528, #10050, #6376, #8320, #14943, #16674, #11248, #9625, #4869, #13212, #8430, #19794, #9729, #128, #21211, #236, #6481, #9833, #16456, #3148, #8211, #9942, #4976, #18274, #3463, #14728, #6805, #12986, #4758, #11354, #5083, #1637, #16352, #14838, #15, #11575, #17951, #21310, #13098, #19684, #18166, #11462, #3363, #448, #1964, #20014, #18382, #12104, #7224, #3571, #7015, #13423, #5502, #10472, #16779, #2274, #20224, #659, #13638, #5190, #13845, #20438, #18696, #5291, #2169, #10363, #3676, #11999, #20331, #7120, #11787, #17093, #11894, #8853, #8752, #13745, #8535, #16880, #15474, #10160, #5393, #15159, #345, #18487, #6910, #10258, #13533, #2064, #8639, #16989, #18589, #15373, #20122, #15266, #3776, #551, #3884, #17917, #8395, #309, #18352, #6878, #19979, #11755, #11322, #3326, #4829, #21388, #5159, #9908, #6666, #19760, #14911, #19871, #5047, #3222, #13392, #8281, #18028, #6554, #8068, #11648, #11542, #3538, #3115, #10126, #13286, #9799, #4943, #8174, #14805, #6447, #6771, #18242, #3434, #13498, #11427, #16747, #10016, #9697, #1935, #16422, #16318, #16640, #1825, #20091, #8501, #21275, #1600, #13174, #15021, #205, #1493, #13063, #15127, #95, #14698, #16529, #18133, #19649, #1714, #9137, #9031, #7189, #8925, #2344, #12613, #20723, #5788, #17059, #15548, #20513, #731, #12394, #7619, #17164, #13812, #3956, #9248, #5577, #7406, #15758, #5897, #15865, #4064, #5682, #7299, #12507, #10438, #2242, #14032, #20402, #19100, #4284, #15437, #2659, #18873, #12182, #20612, #18768, #10543, #18986, #13925, #10648, #17267, #4167, #1054, #946, #7513, #14137, #6004, #10866, #17472, #14246, #20833, #19204, #2772, #9355, #15972, #20935, #14355, #7727, #10971, #6104, #1156, #12717, #4386, #17580, #15359, #6683, #13303, #16545, #13408, #7107, #15038, #16763, #11983, #19997, #13727, #222, #6790, #10350, #10147, #18258, #18577, #19888, #20317, #5489, #5175, #10034, #12089, #9925, #5064, #8734, #1730, #8520, #18473, #11668, #3345, #11772, #3449, #16660, #18367, #1951, #3558, #15146, #328, #5377, #13623, #10243, #1845, #16973, #6895, #8304, #13517, #3762, #540, #8413 ) ),
 .UNSPECIFIED., .F., .F., .T. ) 
 B_SPLINE_SURFACE_WITH_KNOTS ( ( 2, 2 ),
 ( 3, 2, 2, 2, 2, 2, 2, 2, 2, 2, 2, 2, 2, 2, 2, 2, 2, 2, 2, 2, 2, 2, 2, 2, 2, 2, 2, 2, 2, 2, 2, 2, 2, 2, 2, 2, 2, 2, 2, 2, 2, 2, 2, 2, 2, 2, 2, 2, 2, 2, 2, 2, 2, 2, 2, 2, 2, 2, 2, 2, 2, 2, 2, 2, 2, 2, 2, 2, 2, 2, 2, 2, 2, 2, 2, 2, 2, 2, 2, 2, 2, 2, 2, 2, 2, 2, 2, 2, 2, 2, 2, 2, 2, 2, 2, 2, 2, 2, 2, 2, 2, 2, 2, 2, 2, 2, 2, 2, 2, 2, 2, 2, 2, 2, 2, 2, 2, 2, 2, 2, 2, 2, 2, 2, 2, 2, 2, 2, 2, 2, 2, 2, 2, 2, 2, 2, 2, 2, 2, 2, 2, 2, 2, 2, 2, 2, 2, 2, 2, 2, 2, 2, 2, 2, 2, 2, 2, 2, 2, 2, 2, 2, 2, 2, 2, 2, 2, 2, 2, 2, 2, 2, 2, 2, 2, 2, 2, 2, 2, 2, 2, 2, 2, 2, 2, 2, 2, 2, 2, 2, 2, 2, 2, 2, 2, 2, 2, 2, 2, 2, 2, 2, 2, 2, 2, 2, 2, 2, 2, 2, 2, 2, 2, 2, 2, 2, 2, 2, 2, 2, 2, 2, 2, 2, 2, 2, 2, 2, 2, 2, 2, 2, 2, 2, 2, 2, 2, 2, 2, 2, 2, 2, 2, 2, 2, 2, 2, 2, 2, 2, 2, 2, 2, 2, 2, 2, 2, 2, 2, 2, 2, 2, 2, 2, 2, 2, 2, 2, 2, 2, 2, 2, 2, 2, 2, 2, 2, 2, 2, 2, 2, 2, 2, 2, 2, 2, 2, 2, 2, 2, 2, 2, 2, 2, 2, 2, 2, 2, 2, 2, 2, 2, 2, 2, 2, 2, 2, 2, 2, 2, 2, 2, 2, 2, 2, 2, 2, 2, 2, 2, 2, 2, 2, 2, 2, 2, 2, 2, 2, 2, 2, 2, 2, 2, 2, 2, 2, 2, 2, 2, 2, 2, 2, 2, 2, 2, 2, 2, 2, 2, 2, 2, 2, 2, 2, 2, 2, 2, 2, 2, 2, 2, 2, 2, 2, 2, 2, 2, 2, 2, 2, 2, 2, 2, 2, 2, 2, 2, 2, 2, 2, 2, 2, 2, 2, 2, 2, 2, 2, 2, 2, 2, 2, 2, 2, 2, 2, 2, 2, 2, 2, 2, 2, 2, 2, 2, 2, 2, 2, 2, 2, 2, 2, 2, 2, 2, 2, 2, 2, 2, 2, 2, 2, 2, 2, 2, 2, 2, 2, 2, 2, 2, 2, 2, 2, 2, 2, 2, 2, 2, 2, 2, 2, 2, 2, 2, 2, 2, 2, 2, 2, 2, 2, 2, 2, 2, 2, 2, 2, 2, 2, 2, 2, 2, 2, 2, 2, 2, 2, 2, 2, 2, 2, 2, 2, 2, 2, 2, 2, 2, 2, 2, 2, 2, 2, 2, 2, 2, 2, 2, 2, 2, 2, 2, 2, 2, 2, 2, 2, 2, 2, 2, 2, 3 ),
 ( 0.000000000000000000, 1.000000000000000000 ),
 ( 0.000000000000000000, 0.001953125000000000000, 0.003906250000000000000, 0.005859375000000000000, 0.007812500000000000000, 0.009765625000000000000, 0.01171875000000000000, 0.01367187500000000000, 0.01562500000000000000, 0.01757812500000000000, 0.01953125000000000000, 0.02148437500000000000, 0.02343750000000000000, 0.02539062500000000000, 0.02734375000000000000, 0.02929687500000000000, 0.03125000000000000000, 0.03320312500000000000, 0.03515625000000000000, 0.03710937500000000000, 0.03906250000000000000, 0.04101562500000000000, 0.04296875000000000000, 0.04492187500000000000, 0.04687500000000000000, 0.04882812500000000000, 0.05078125000000000000, 0.05273437500000000000, 0.05468750000000000000, 0.05664062500000000000, 0.05859375000000000000, 0.06054687500000000000, 0.06250000000000000000, 0.06445312500000000000, 0.06640625000000000000, 0.06835937500000000000, 0.07031250000000000000, 0.07226562500000000000, 0.07421875000000000000, 0.07617187500000000000, 0.07812500000000000000, 0.08007812500000000000, 0.08203125000000000000, 0.08398437500000000000, 0.08593750000000000000, 0.08789062500000000000, 0.08984375000000000000, 0.09179687500000000000, 0.09375000000000000000, 0.09570312500000000000, 0.09765625000000000000, 0.09960937500000000000, 0.1015625000000000000, 0.1035156250000000000, 0.1054687500000000000, 0.1074218750000000000, 0.1093750000000000000, 0.1113281250000000000, 0.1132812500000000000, 0.1152343750000000000, 0.1171875000000000000, 0.1191406250000000000, 0.1210937500000000000, 0.1230468750000000000, 0.1250000000000000000, 0.1269531250000000000, 0.1289062500000000000, 0.1308593750000000000, 0.1328125000000000000, 0.1347656250000000000, 0.1367187500000000000, 0.1386718750000000000, 0.1406250000000000000, 0.1425781250000000000, 0.1445312500000000000, 0.1464843750000000000, 0.1484375000000000000, 0.1503906250000000000, 0.1523437500000000000, 0.1542968750000000000, 0.1562500000000000000, 0.1582031250000000000, 0.1601562500000000000, 0.1621093750000000000, 0.1640625000000000000, 0.1660156250000000000, 0.1679687500000000000, 0.1699218750000000000, 0.1718750000000000000, 0.1738281250000000000, 0.1757812500000000000, 0.1777343750000000000, 0.1796875000000000000, 0.1816406250000000000, 0.1835937500000000000, 0.1855468750000000000, 0.1875000000000000000, 0.1894531250000000000, 0.1914062500000000000, 0.1933593750000000000, 0.1953125000000000000, 0.1972656250000000000, 0.1992187500000000000, 0.2011718750000000000, 0.2031250000000000000, 0.2050781250000000000, 0.2070312500000000000, 0.2089843750000000000, 0.2109375000000000000, 0.2128906250000000000, 0.2148437500000000000, 0.2167968750000000000, 0.2187500000000000000, 0.2207031250000000000, 0.2226562500000000000, 0.2246093750000000000, 0.2265625000000000000, 0.2285156250000000000, 0.2304687500000000000, 0.2324218750000000000, 0.2343750000000000000, 0.2363281250000000000, 0.2382812500000000000, 0.2402343750000000000, 0.2421875000000000000, 0.2441406250000000000, 0.2460937500000000000, 0.2480468750000000000, 0.2500000000000000000, 0.2519531250000000000, 0.2539062500000000000, 0.2558593750000000000, 0.2578125000000000000, 0.2597656250000000000, 0.2617187500000000000, 0.2636718750000000000, 0.2656250000000000000, 0.2675781250000000000, 0.2695312500000000000, 0.2714843750000000000, 0.2734375000000000000, 0.2753906250000000000, 0.2773437500000000000, 0.2792968750000000000, 0.2812500000000000000, 0.2832031250000000000, 0.2851562500000000000, 0.2871093750000000000, 0.2890625000000000000, 0.2910156250000000000, 0.2929687500000000000, 0.2949218750000000000, 0.2968750000000000000, 0.2988281250000000000, 0.3007812500000000000, 0.3027343750000000000, 0.3046875000000000000, 0.3066406250000000000, 0.3085937500000000000, 0.3105468750000000000, 0.3125000000000000000, 0.3144531250000000000, 0.3164062500000000000, 0.3183593750000000000, 0.3203125000000000000, 0.3222656250000000000, 0.3242187500000000000, 0.3261718750000000000, 0.3281250000000000000, 0.3300781250000000000, 0.3320312500000000000, 0.3339843750000000000, 0.3359375000000000000, 0.3378906250000000000, 0.3398437500000000000, 0.3417968750000000000, 0.3437500000000000000, 0.3457031250000000000, 0.3476562500000000000, 0.3496093750000000000, 0.3515625000000000000, 0.3535156250000000000, 0.3554687500000000000, 0.3574218750000000000, 0.3593750000000000000, 0.3613281250000000000, 0.3632812500000000000, 0.3652343750000000000, 0.3671875000000000000, 0.3691406250000000000, 0.3710937500000000000, 0.3730468750000000000, 0.3750000000000000000, 0.3769531250000000000, 0.3789062500000000000, 0.3808593750000000000, 0.3828125000000000000, 0.3847656250000000000, 0.3867187500000000000, 0.3886718750000000000, 0.3906250000000000000, 0.3925781250000000000, 0.3945312500000000000, 0.3964843750000000000, 0.3984375000000000000, 0.4003906250000000000, 0.4023437500000000000, 0.4042968750000000000, 0.4062500000000000000, 0.4082031250000000000, 0.4101562500000000000, 0.4121093750000000000, 0.4140625000000000000, 0.4160156250000000000, 0.4179687500000000000, 0.4199218750000000000, 0.4218750000000000000, 0.4238281250000000000, 0.4257812500000000000, 0.4277343750000000000, 0.4296875000000000000, 0.4316406250000000000, 0.4335937500000000000, 0.4355468750000000000, 0.4375000000000000000, 0.4394531250000000000, 0.4414062500000000000, 0.4433593750000000000, 0.4453125000000000000, 0.4472656250000000000, 0.4492187500000000000, 0.4511718750000000000, 0.4531250000000000000, 0.4550781250000000000, 0.4570312500000000000, 0.4589843750000000000, 0.4609375000000000000, 0.4628906250000000000, 0.4648437500000000000, 0.4667968750000000000, 0.4687500000000000000, 0.4707031250000000000, 0.4726562500000000000, 0.4746093750000000000, 0.4765625000000000000, 0.4785156250000000000, 0.4804687500000000000, 0.4824218750000000000, 0.4843750000000000000, 0.4863281250000000000, 0.4882812500000000000, 0.4902343750000000000, 0.4921875000000000000, 0.4941406250000000000, 0.4960937500000000000, 0.4980468750000000000, 0.5000000000000000000, 0.5019531250000000000, 0.5039062500000000000, 0.5058593750000000000, 0.5078125000000000000, 0.5097656250000000000, 0.5117187500000000000, 0.5136718750000000000, 0.5156250000000000000, 0.5175781250000000000, 0.5195312500000000000, 0.5214843750000000000, 0.5234375000000000000, 0.5253906250000000000, 0.5273437500000000000, 0.5292968750000000000, 0.5312500000000000000, 0.5332031250000000000, 0.5351562500000000000, 0.5371093750000000000, 0.5390625000000000000, 0.5410156250000000000, 0.5429687500000000000, 0.5449218750000000000, 0.5468750000000000000, 0.5488281250000000000, 0.5507812500000000000, 0.5527343750000000000, 0.5546875000000000000, 0.5566406250000000000, 0.5585937500000000000, 0.5605468750000000000, 0.5625000000000000000, 0.5644531250000000000, 0.5664062500000000000, 0.5683593750000000000, 0.5703125000000000000, 0.5722656250000000000, 0.5742187500000000000, 0.5761718750000000000, 0.5781250000000000000, 0.5800781250000000000, 0.5820312500000000000, 0.5839843750000000000, 0.5859375000000000000, 0.5878906250000000000, 0.5898437500000000000, 0.5917968750000000000, 0.5937500000000000000, 0.5957031250000000000, 0.5976562500000000000, 0.5996093750000000000, 0.6015625000000000000, 0.6035156250000000000, 0.6054687500000000000, 0.6074218750000000000, 0.6093750000000000000, 0.6113281250000000000, 0.6132812500000000000, 0.6152343750000000000, 0.6171875000000000000, 0.6191406250000000000, 0.6210937500000000000, 0.6230468750000000000, 0.6250000000000000000, 0.6269531250000000000, 0.6289062500000000000, 0.6308593750000000000, 0.6328125000000000000, 0.6347656250000000000, 0.6367187500000000000, 0.6386718750000000000, 0.6406250000000000000, 0.6425781250000000000, 0.6445312500000000000, 0.6464843750000000000, 0.6484375000000000000, 0.6503906250000000000, 0.6523437500000000000, 0.6542968750000000000, 0.6562500000000000000, 0.6582031250000000000, 0.6601562500000000000, 0.6621093750000000000, 0.6640625000000000000, 0.6660156250000000000, 0.6679687500000000000, 0.6699218750000000000, 0.6718750000000000000, 0.6738281250000000000, 0.6757812500000000000, 0.6777343750000000000, 0.6796875000000000000, 0.6816406250000000000, 0.6835937500000000000, 0.6855468750000000000, 0.6875000000000000000, 0.6894531250000000000, 0.6914062500000000000, 0.6933593750000000000, 0.6953125000000000000, 0.6972656250000000000, 0.6992187500000000000, 0.7011718750000000000, 0.7031250000000000000, 0.7050781250000000000, 0.7070312500000000000, 0.7089843750000000000, 0.7109375000000000000, 0.7128906250000000000, 0.7148437500000000000, 0.7167968750000000000, 0.7187500000000000000, 0.7207031250000000000, 0.7226562500000000000, 0.7246093750000000000, 0.7265625000000000000, 0.7285156250000000000, 0.7304687500000000000, 0.7324218750000000000, 0.7343750000000000000, 0.7363281250000000000, 0.7382812500000000000, 0.7402343750000000000, 0.7421875000000000000, 0.7441406250000000000, 0.7460937500000000000, 0.7480468750000000000, 0.7500000000000000000, 0.7519531250000000000, 0.7539062500000000000, 0.7558593750000000000, 0.7578125000000000000, 0.7597656250000000000, 0.7617187500000000000, 0.7636718750000000000, 0.7656250000000000000, 0.7675781250000000000, 0.7695312500000000000, 0.7714843750000000000, 0.7734375000000000000, 0.7753906250000000000, 0.7773437500000000000, 0.7792968750000000000, 0.7812500000000000000, 0.7832031250000000000, 0.7851562500000000000, 0.7871093750000000000, 0.7890625000000000000, 0.7910156250000000000, 0.7929687500000000000, 0.7949218750000000000, 0.7968750000000000000, 0.7988281250000000000, 0.8007812500000000000, 0.8027343750000000000, 0.8046875000000000000, 0.8066406250000000000, 0.8085937500000000000, 0.8105468750000000000, 0.8125000000000000000, 0.8144531250000000000, 0.8164062500000000000, 0.8183593750000000000, 0.8203125000000000000, 0.8222656250000000000, 0.8242187500000000000, 0.8261718750000000000, 0.8281250000000000000, 0.8300781250000000000, 0.8320312500000000000, 0.8339843750000000000, 0.8359375000000000000, 0.8378906250000000000, 0.8398437500000000000, 0.8417968750000000000, 0.8437500000000000000, 0.8457031250000000000, 0.8476562500000000000, 0.8496093750000000000, 0.8515625000000000000, 0.8535156250000000000, 0.8554687500000000000, 0.8574218750000000000, 0.8593750000000000000, 0.8613281250000000000, 0.8632812500000000000, 0.8652343750000000000, 0.8671875000000000000, 0.8691406250000000000, 0.8710937500000000000, 0.8730468750000000000, 0.8750000000000000000, 0.8769531250000000000, 0.8789062500000000000, 0.8808593750000000000, 0.8828125000000000000, 0.8847656250000000000, 0.8867187500000000000, 0.8886718750000000000, 0.8906250000000000000, 0.8925781250000000000, 0.8945312500000000000, 0.8964843750000000000, 0.8984375000000000000, 0.9003906250000000000, 0.9023437500000000000, 0.9042968750000000000, 0.9062500000000000000, 0.9082031250000000000, 0.9101562500000000000, 0.9121093750000000000, 0.9140625000000000000, 0.9160156250000000000, 0.9179687500000000000, 0.9199218750000000000, 0.9218750000000000000, 0.9238281250000000000, 0.9257812500000000000, 0.9277343750000000000, 0.9296875000000000000, 0.9316406250000000000, 0.9335937500000000000, 0.9355468750000000000, 0.9375000000000000000, 0.9394531250000000000, 0.9414062500000000000, 0.9433593750000000000, 0.9453125000000000000, 0.9472656250000000000, 0.9492187500000000000, 0.9511718750000000000, 0.9531250000000000000, 0.9550781250000000000, 0.9570312500000000000, 0.9589843750000000000, 0.9609375000000000000, 0.9628906250000000000, 0.9648437500000000000, 0.9667968750000000000, 0.9687500000000000000, 0.9707031250000000000, 0.9726562500000000000, 0.9746093750000000000, 0.9765625000000000000, 0.9785156250000000000, 0.9791718336226143959, 0.9889635519588405588 ),
 .UNSPECIFIED. ) 
 GEOMETRIC_REPRESENTATION_ITEM ( )  RATIONAL_B_SPLINE_SURFACE ( (
 ( 1.000000000000000000, 0.9807852804032304306, 1.000000000000000000, 0.9807852804032304306, 1.000000000000000000, 0.9807852804032304306, 1.000000000000000000, 0.9807852804032304306, 1.000000000000000000, 0.9807852804032304306, 1.000000000000000000, 0.9807852804032304306, 1.000000000000000000, 0.9807852804032304306, 1.000000000000000000, 0.9807852804032304306, 1.000000000000000000, 0.9807852804032304306, 1.000000000000000000, 0.9807852804032304306, 1.000000000000000000, 0.9807852804032304306, 1.000000000000000000, 0.9807852804032304306, 1.000000000000000000, 0.9807852804032304306, 1.000000000000000000, 0.9807852804032304306, 1.000000000000000000, 0.9807852804032304306, 1.000000000000000000, 0.9807852804032304306, 1.000000000000000000, 0.9807852804032304306, 1.000000000000000000, 0.9807852804032304306, 1.000000000000000000, 0.9807852804032304306, 1.000000000000000000, 0.9807852804032304306, 1.000000000000000000, 0.9807852804032304306, 1.000000000000000000, 0.9807852804032304306, 1.000000000000000000, 0.9807852804032304306, 1.000000000000000000, 0.9807852804032304306, 1.000000000000000000, 0.9807852804032304306, 1.000000000000000000, 0.9807852804032304306, 1.000000000000000000, 0.9807852804032304306, 1.000000000000000000, 0.9807852804032304306, 1.000000000000000000, 0.9807852804032304306, 1.000000000000000000, 0.9807852804032304306, 1.000000000000000000, 0.9807852804032304306, 1.000000000000000000, 0.9807852804032304306, 1.000000000000000000, 0.9807852804032304306, 1.000000000000000000, 0.9807852804032304306, 1.000000000000000000, 0.9807852804032304306, 1.000000000000000000, 0.9807852804032304306, 1.000000000000000000, 0.9807852804032304306, 1.000000000000000000, 0.9807852804032304306, 1.000000000000000000, 0.9807852804032304306, 1.000000000000000000, 0.9807852804032304306, 1.000000000000000000, 0.9807852804032304306, 1.000000000000000000, 0.9807852804032304306, 1.000000000000000000, 0.9807852804032304306, 1.000000000000000000, 0.9807852804032304306, 1.000000000000000000, 0.9807852804032304306, 1.000000000000000000, 0.9807852804032304306, 1.000000000000000000, 0.9807852804032304306, 1.000000000000000000, 0.9807852804032304306, 1.000000000000000000, 0.9807852804032304306, 1.000000000000000000, 0.9807852804032304306, 1.000000000000000000, 0.9807852804032304306, 1.000000000000000000, 0.9807852804032304306, 1.000000000000000000, 0.9807852804032304306, 1.000000000000000000, 0.9807852804032304306, 1.000000000000000000, 0.9807852804032304306, 1.000000000000000000, 0.9807852804032304306, 1.000000000000000000, 0.9807852804032304306, 1.000000000000000000, 0.9807852804032304306, 1.000000000000000000, 0.9807852804032304306, 1.000000000000000000, 0.9807852804032304306, 1.000000000000000000, 0.9807852804032304306, 1.000000000000000000, 0.9807852804032304306, 1.000000000000000000, 0.9807852804032304306, 1.000000000000000000, 0.9807852804032304306, 1.000000000000000000, 0.9807852804032304306, 1.000000000000000000, 0.9807852804032304306, 1.000000000000000000, 0.9807852804032304306, 1.000000000000000000, 0.9807852804032304306, 1.000000000000000000, 0.9807852804032304306, 1.000000000000000000, 0.9807852804032304306, 1.000000000000000000, 0.9807852804032304306, 1.000000000000000000, 0.9807852804032304306, 1.000000000000000000, 0.9807852804032304306, 1.000000000000000000, 0.9807852804032304306, 1.000000000000000000, 0.9807852804032304306, 1.000000000000000000, 0.9807852804032304306, 1.000000000000000000, 0.9807852804032304306, 1.000000000000000000, 0.9807852804032304306, 1.000000000000000000, 0.9807852804032304306, 1.000000000000000000, 0.9807852804032304306, 1.000000000000000000, 0.9807852804032304306, 1.000000000000000000, 0.9807852804032304306, 1.000000000000000000, 0.9807852804032304306, 1.000000000000000000, 0.9807852804032304306, 1.000000000000000000, 0.9807852804032304306, 1.000000000000000000, 0.9807852804032304306, 1.000000000000000000, 0.9807852804032304306, 1.000000000000000000, 0.9807852804032304306, 1.000000000000000000, 0.9807852804032304306, 1.000000000000000000, 0.9807852804032304306, 1.000000000000000000, 0.9807852804032304306, 1.000000000000000000, 0.9807852804032304306, 1.000000000000000000, 0.9807852804032304306, 1.000000000000000000, 0.9807852804032304306, 1.000000000000000000, 0.9807852804032304306, 1.000000000000000000, 0.9807852804032304306, 1.000000000000000000, 0.9807852804032304306, 1.000000000000000000, 0.9807852804032304306, 1.000000000000000000, 0.9807852804032304306, 1.000000000000000000, 0.9807852804032304306, 1.000000000000000000, 0.9807852804032304306, 1.000000000000000000, 0.9807852804032304306, 1.000000000000000000, 0.9807852804032304306, 1.000000000000000000, 0.9807852804032304306, 1.000000000000000000, 0.9807852804032304306, 1.000000000000000000, 0.9807852804032304306, 1.000000000000000000, 0.9807852804032304306, 1.000000000000000000, 0.9807852804032304306, 1.000000000000000000, 0.9807852804032304306, 1.000000000000000000, 0.9807852804032304306, 1.000000000000000000, 0.9807852804032304306, 1.000000000000000000, 0.9807852804032304306, 1.000000000000000000, 0.9807852804032304306, 1.000000000000000000, 0.9807852804032304306, 1.000000000000000000, 0.9807852804032304306, 1.000000000000000000, 0.9807852804032304306, 1.000000000000000000, 0.9807852804032304306, 1.000000000000000000, 0.9807852804032304306, 1.000000000000000000, 0.9807852804032304306, 1.000000000000000000, 0.9807852804032304306, 1.000000000000000000, 0.9807852804032304306, 1.000000000000000000, 0.9807852804032304306, 1.000000000000000000, 0.9807852804032304306, 1.000000000000000000, 0.9807852804032304306, 1.000000000000000000, 0.9807852804032304306, 1.000000000000000000, 0.9807852804032304306, 1.000000000000000000, 0.9807852804032304306, 1.000000000000000000, 0.9807852804032304306, 1.000000000000000000, 0.9807852804032304306, 1.000000000000000000, 0.9807852804032304306, 1.000000000000000000, 0.9807852804032304306, 1.000000000000000000, 0.9807852804032304306, 1.000000000000000000, 0.9807852804032304306, 1.000000000000000000, 0.9807852804032304306, 1.000000000000000000, 0.9807852804032304306, 1.000000000000000000, 0.9807852804032304306, 1.000000000000000000, 0.9807852804032304306, 1.000000000000000000, 0.9807852804032304306, 1.000000000000000000, 0.9807852804032304306, 1.000000000000000000, 0.9807852804032304306, 1.000000000000000000, 0.9807852804032304306, 1.000000000000000000, 0.9807852804032304306, 1.000000000000000000, 0.9807852804032304306, 1.000000000000000000, 0.9807852804032304306, 1.000000000000000000, 0.9807852804032304306, 1.000000000000000000, 0.9807852804032304306, 1.000000000000000000, 0.9807852804032304306, 1.000000000000000000, 0.9807852804032304306, 1.000000000000000000, 0.9807852804032304306, 1.000000000000000000, 0.9807852804032304306, 1.000000000000000000, 0.9807852804032304306, 1.000000000000000000, 0.9807852804032304306, 1.000000000000000000, 0.9807852804032304306, 1.000000000000000000, 0.9807852804032304306, 1.000000000000000000, 0.9807852804032304306, 1.000000000000000000, 0.9807852804032304306, 1.000000000000000000, 0.9807852804032304306, 1.000000000000000000, 0.9807852804032304306, 1.000000000000000000, 0.9807852804032304306, 1.000000000000000000, 0.9807852804032304306, 1.000000000000000000, 0.9807852804032304306, 1.000000000000000000, 0.9807852804032304306, 1.000000000000000000, 0.9807852804032304306, 1.000000000000000000, 0.9807852804032304306, 1.000000000000000000, 0.9807852804032304306, 1.000000000000000000, 0.9807852804032304306, 1.000000000000000000, 0.9807852804032304306, 1.000000000000000000, 0.9807852804032304306, 1.000000000000000000, 0.9807852804032304306, 1.000000000000000000, 0.9807852804032304306, 1.000000000000000000, 0.9807852804032304306, 1.000000000000000000, 0.9807852804032304306, 1.000000000000000000, 0.9807852804032304306, 1.000000000000000000, 0.9807852804032304306, 1.000000000000000000, 0.9807852804032304306, 1.000000000000000000, 0.9807852804032304306, 1.000000000000000000, 0.9807852804032304306, 1.000000000000000000, 0.9807852804032304306, 1.000000000000000000, 0.9807852804032304306, 1.000000000000000000, 0.9807852804032304306, 1.000000000000000000, 0.9807852804032304306, 1.000000000000000000, 0.9807852804032304306, 1.000000000000000000, 0.9807852804032304306, 1.000000000000000000, 0.9807852804032304306, 1.000000000000000000, 0.9807852804032304306, 1.000000000000000000, 0.9807852804032304306, 1.000000000000000000, 0.9807852804032304306, 1.000000000000000000, 0.9807852804032304306, 1.000000000000000000, 0.9807852804032304306, 1.000000000000000000, 0.9807852804032304306, 1.000000000000000000, 0.9807852804032304306, 1.000000000000000000, 0.9807852804032304306, 1.000000000000000000, 0.9807852804032304306, 1.000000000000000000, 0.9807852804032304306, 1.000000000000000000, 0.9807852804032304306, 1.000000000000000000, 0.9807852804032304306, 1.000000000000000000, 0.9807852804032304306, 1.000000000000000000, 0.9807852804032304306, 1.000000000000000000, 0.9807852804032304306, 1.000000000000000000, 0.9807852804032304306, 1.000000000000000000, 0.9807852804032304306, 1.000000000000000000, 0.9807852804032304306, 1.000000000000000000, 0.9807852804032304306, 1.000000000000000000, 0.9807852804032304306, 1.000000000000000000, 0.9807852804032304306, 1.000000000000000000, 0.9807852804032304306, 1.000000000000000000, 0.9807852804032304306, 1.000000000000000000, 0.9807852804032304306, 1.000000000000000000, 0.9807852804032304306, 1.000000000000000000, 0.9807852804032304306, 1.000000000000000000, 0.9807852804032304306, 1.000000000000000000, 0.9807852804032304306, 1.000000000000000000, 0.9807852804032304306, 1.000000000000000000, 0.9807852804032304306, 1.000000000000000000, 0.9807852804032304306, 1.000000000000000000, 0.9807852804032304306, 1.000000000000000000, 0.9807852804032304306, 1.000000000000000000, 0.9807852804032304306, 1.000000000000000000, 0.9807852804032304306, 1.000000000000000000, 0.9807852804032304306, 1.000000000000000000, 0.9807852804032304306, 1.000000000000000000, 0.9807852804032304306, 1.000000000000000000, 0.9807852804032304306, 1.000000000000000000, 0.9807852804032304306, 1.000000000000000000, 0.9807852804032304306, 1.000000000000000000, 0.9807852804032304306, 1.000000000000000000, 0.9807852804032304306, 1.000000000000000000, 0.9807852804032304306, 1.000000000000000000, 0.9807852804032304306, 1.000000000000000000, 0.9807852804032304306, 1.000000000000000000, 0.9807852804032304306, 1.000000000000000000, 0.9807852804032304306, 1.000000000000000000, 0.9807852804032304306, 1.000000000000000000, 0.9807852804032304306, 1.000000000000000000, 0.9807852804032304306, 1.000000000000000000, 0.9807852804032304306, 1.000000000000000000, 0.9807852804032304306, 1.000000000000000000, 0.9807852804032304306, 1.000000000000000000, 0.9807852804032304306, 1.000000000000000000, 0.9807852804032304306, 1.000000000000000000, 0.9807852804032304306, 1.000000000000000000, 0.9807852804032304306, 1.000000000000000000, 0.9807852804032304306, 1.000000000000000000, 0.9807852804032304306, 1.000000000000000000, 0.9807852804032304306, 1.000000000000000000, 0.9807852804032304306, 1.000000000000000000, 0.9807852804032304306, 1.000000000000000000, 0.9807852804032304306, 1.000000000000000000, 0.9807852804032304306, 1.000000000000000000, 0.9807852804032304306, 1.000000000000000000, 0.9807852804032304306, 1.000000000000000000, 0.9807852804032304306, 1.000000000000000000, 0.9807852804032304306, 1.000000000000000000, 0.9807852804032304306, 1.000000000000000000, 0.9807852804032304306, 1.000000000000000000, 0.9807852804032304306, 1.000000000000000000, 0.9807852804032304306, 1.000000000000000000, 0.9807852804032304306, 1.000000000000000000, 0.9807852804032304306, 1.000000000000000000, 0.9807852804032304306, 1.000000000000000000, 0.9807852804032304306, 1.000000000000000000, 0.9807852804032304306, 1.000000000000000000, 0.9807852804032304306, 1.000000000000000000, 0.9807852804032304306, 1.000000000000000000, 0.9807852804032304306, 1.000000000000000000, 0.9807852804032304306, 1.000000000000000000, 0.9807852804032304306, 1.000000000000000000, 0.9807852804032304306, 1.000000000000000000, 0.9807852804032304306, 1.000000000000000000, 0.9807852804032304306, 1.000000000000000000, 0.9807852804032304306, 1.000000000000000000, 0.9807852804032304306, 1.000000000000000000, 0.9807852804032304306, 1.000000000000000000, 0.9807852804032304306, 1.000000000000000000, 0.9807852804032304306, 1.000000000000000000, 0.9807852804032304306, 1.000000000000000000, 0.9807852804032304306, 1.000000000000000000, 0.9807852804032304306, 1.000000000000000000, 0.9807852804032304306, 1.000000000000000000, 0.9807852804032304306, 1.000000000000000000, 0.9807852804032304306, 1.000000000000000000, 0.9807852804032304306, 1.000000000000000000, 0.9807852804032304306, 1.000000000000000000, 0.9807852804032304306, 1.000000000000000000, 0.9807852804032304306, 1.000000000000000000, 0.9807852804032304306, 1.000000000000000000, 0.9807852804032304306, 1.000000000000000000, 0.9807852804032304306, 1.000000000000000000, 0.9807852804032304306, 1.000000000000000000, 0.9807852804032304306, 1.000000000000000000, 0.9807852804032304306, 1.000000000000000000, 0.9807852804032304306, 1.000000000000000000, 0.9807852804032304306, 1.000000000000000000, 0.9807852804032304306, 1.000000000000000000, 0.9807852804032304306, 1.000000000000000000, 0.9807852804032304306, 1.000000000000000000, 0.9807852804032304306, 1.000000000000000000, 0.9807852804032304306, 1.000000000000000000, 0.9807852804032304306, 1.000000000000000000, 0.9807852804032304306, 1.000000000000000000, 0.9807852804032304306, 1.000000000000000000, 0.9807852804032304306, 1.000000000000000000, 0.9807852804032304306, 1.000000000000000000, 0.9807852804032304306, 1.000000000000000000, 0.9807852804032304306, 1.000000000000000000, 0.9807852804032304306, 1.000000000000000000, 0.9807852804032304306, 1.000000000000000000, 0.9807852804032304306, 1.000000000000000000, 0.9807852804032304306, 1.000000000000000000, 0.9807852804032304306, 1.000000000000000000, 0.9807852804032304306, 1.000000000000000000, 0.9807852804032304306, 1.000000000000000000, 0.9807852804032304306, 1.000000000000000000, 0.9807852804032304306, 1.000000000000000000, 0.9807852804032304306, 1.000000000000000000, 0.9807852804032304306, 1.000000000000000000, 0.9807852804032304306, 1.000000000000000000, 0.9807852804032304306, 1.000000000000000000, 0.9807852804032304306, 1.000000000000000000, 0.9807852804032304306, 1.000000000000000000, 0.9807852804032304306, 1.000000000000000000, 0.9807852804032304306, 1.000000000000000000, 0.9807852804032304306, 1.000000000000000000, 0.9807852804032304306, 1.000000000000000000, 0.9807852804032304306, 1.000000000000000000, 0.9807852804032304306, 1.000000000000000000, 0.9807852804032304306, 1.000000000000000000, 0.9807852804032304306, 1.000000000000000000, 0.9807852804032304306, 1.000000000000000000, 0.9807852804032304306, 1.000000000000000000, 0.9807852804032304306, 1.000000000000000000, 0.9807852804032304306, 1.000000000000000000, 0.9807852804032304306, 1.000000000000000000, 0.9807852804032304306, 1.000000000000000000, 0.9807852804032304306, 1.000000000000000000, 0.9807852804032304306, 1.000000000000000000, 0.9807852804032304306, 1.000000000000000000, 0.9807852804032304306, 1.000000000000000000, 0.9807852804032304306, 1.000000000000000000, 0.9807852804032304306, 1.000000000000000000, 0.9807852804032304306, 1.000000000000000000, 0.9807852804032304306, 1.000000000000000000, 0.9807852804032304306, 1.000000000000000000, 0.9807852804032304306, 1.000000000000000000, 0.9807852804032304306, 1.000000000000000000, 0.9807852804032304306, 1.000000000000000000, 0.9807852804032304306, 1.000000000000000000, 0.9807852804032304306, 1.000000000000000000, 0.9807852804032304306, 1.000000000000000000, 0.9807852804032304306, 1.000000000000000000, 0.9807852804032304306, 1.000000000000000000, 0.9807852804032304306, 1.000000000000000000, 0.9807852804032304306, 1.000000000000000000, 0.9807852804032304306, 1.000000000000000000, 0.9807852804032304306, 1.000000000000000000, 0.9807852804032304306, 1.000000000000000000, 0.9807852804032304306, 1.000000000000000000, 0.9807852804032304306, 1.000000000000000000, 0.9807852804032304306, 1.000000000000000000, 0.9807852804032304306, 1.000000000000000000, 0.9807852804032304306, 1.000000000000000000, 0.9807852804032304306, 1.000000000000000000, 0.9807852804032304306, 1.000000000000000000, 0.9807852804032304306, 1.000000000000000000, 0.9807852804032304306, 1.000000000000000000, 0.9807852804032304306, 1.000000000000000000, 0.9807852804032304306, 1.000000000000000000, 0.9807852804032304306, 1.000000000000000000, 0.9807852804032304306, 1.000000000000000000, 0.9807852804032304306, 1.000000000000000000, 0.9807852804032304306, 1.000000000000000000, 0.9807852804032304306, 1.000000000000000000, 0.9807852804032304306, 1.000000000000000000, 0.9807852804032304306, 1.000000000000000000, 0.9807852804032304306, 1.000000000000000000, 0.9807852804032304306, 1.000000000000000000, 0.9807852804032304306, 1.000000000000000000, 0.9807852804032304306, 1.000000000000000000, 0.9807852804032304306, 1.000000000000000000, 0.9807852804032304306, 1.000000000000000000, 0.9807852804032304306, 1.000000000000000000, 0.9807852804032304306, 1.000000000000000000, 0.9807852804032304306, 1.000000000000000000, 0.9807852804032304306, 1.000000000000000000, 0.9807852804032304306, 1.000000000000000000, 0.9807852804032304306, 1.000000000000000000, 0.9807852804032304306, 1.000000000000000000, 0.9807852804032304306, 1.000000000000000000, 0.9807852804032304306, 1.000000000000000000, 0.9807852804032304306, 1.000000000000000000, 0.9807852804032304306, 1.000000000000000000, 0.9807852804032304306, 1.000000000000000000, 0.9807852804032304306, 1.000000000000000000, 0.9807852804032304306, 1.000000000000000000, 0.9807852804032304306, 1.000000000000000000, 0.9807852804032304306, 1.000000000000000000, 0.9807852804032304306, 1.000000000000000000, 0.9807852804032304306, 1.000000000000000000, 0.9807852804032304306, 1.000000000000000000, 0.9807852804032304306, 1.000000000000000000, 0.9807852804032304306, 1.000000000000000000, 0.9807852804032304306, 1.000000000000000000, 0.9807852804032304306, 1.000000000000000000, 0.9807852804032304306, 1.000000000000000000, 0.9807852804032304306, 1.000000000000000000, 0.9807852804032304306, 1.000000000000000000, 0.9807852804032304306, 1.000000000000000000, 0.9807852804032304306, 1.000000000000000000, 0.9807852804032304306, 1.000000000000000000, 0.9807852804032304306, 1.000000000000000000, 0.9807852804032304306, 1.000000000000000000, 0.9807852804032304306, 1.000000000000000000, 0.9807852804032304306, 1.000000000000000000, 0.9807852804032304306, 1.000000000000000000, 0.9807852804032304306, 1.000000000000000000, 0.9807852804032304306, 1.000000000000000000, 0.9807852804032304306, 1.000000000000000000, 0.9807852804032304306, 1.000000000000000000, 0.9807852804032304306, 1.000000000000000000, 0.9807852804032304306, 1.000000000000000000, 0.9807852804032304306, 1.000000000000000000, 0.9807852804032304306, 1.000000000000000000, 0.9807852804032304306, 1.000000000000000000, 0.9807852804032304306, 1.000000000000000000, 0.9807852804032304306, 1.000000000000000000, 0.9807852804032304306, 1.000000000000000000, 0.9807852804032304306, 1.000000000000000000, 0.9807852804032304306, 1.000000000000000000, 0.9807852804032304306, 1.000000000000000000, 0.9807852804032304306, 1.000000000000000000, 0.9807852804032304306, 1.000000000000000000, 0.9807852804032304306, 1.000000000000000000, 0.9807852804032304306, 1.000000000000000000, 0.9807852804032304306, 1.000000000000000000, 0.9807852804032304306, 1.000000000000000000, 0.9807852804032304306, 1.000000000000000000, 0.9807852804032304306, 1.000000000000000000, 0.9807852804032304306, 1.000000000000000000, 0.9807852804032304306, 1.000000000000000000, 0.9807852804032304306, 1.000000000000000000, 0.9807852804032304306, 1.000000000000000000, 0.9807852804032304306, 1.000000000000000000, 0.9807852804032304306, 1.000000000000000000, 0.9807852804032304306, 1.000000000000000000, 0.9807852804032304306, 1.000000000000000000, 0.9807852804032304306, 1.000000000000000000, 0.9807852804032304306, 1.000000000000000000, 0.9807852804032304306, 1.000000000000000000, 0.9807852804032304306, 1.000000000000000000, 0.9807852804032304306, 1.000000000000000000, 0.9807852804032304306, 1.000000000000000000, 0.9807852804032304306, 1.000000000000000000, 0.9807852804032304306, 1.000000000000000000, 0.9807852804032304306, 1.000000000000000000, 0.9807852804032304306, 1.000000000000000000, 0.9807852804032304306, 1.000000000000000000, 0.9807852804032304306, 1.000000000000000000, 0.9807852804032304306, 1.000000000000000000, 0.9807852804032304306, 1.000000000000000000, 0.9807852804032304306, 1.000000000000000000, 0.9807852804032304306, 1.000000000000000000, 0.9807852804032304306, 1.000000000000000000, 0.9807852804032304306, 1.000000000000000000, 0.9807852804032304306, 1.000000000000000000, 0.9807852804032304306, 1.000000000000000000, 0.9807852804032304306, 1.000000000000000000, 0.9807852804032304306, 1.000000000000000000, 0.9807852804032304306, 1.000000000000000000, 0.9807852804032304306, 1.000000000000000000, 0.9807852804032304306, 1.000000000000000000, 0.9807852804032304306, 1.000000000000000000, 0.9807852804032304306, 1.000000000000000000, 0.9807852804032304306, 1.000000000000000000, 0.9807852804032304306, 1.000000000000000000, 0.9807852804032304306, 1.000000000000000000, 0.9807852804032304306, 1.000000000000000000, 0.9807852804032304306, 1.000000000000000000, 0.9807852804032304306, 1.000000000000000000, 0.9807852804032304306, 1.000000000000000000, 0.9807852804032304306, 1.000000000000000000, 0.9807852804032304306, 1.000000000000000000, 0.9807852804032304306, 1.000000000000000000, 0.9807852804032304306, 1.000000000000000000, 0.9807852804032304306, 1.000000000000000000, 0.9807852804032304306, 1.000000000000000000, 0.9807852804032304306, 1.000000000000000000, 0.9807852804032304306, 1.000000000000000000, 0.9807852804032304306, 1.000000000000000000, 0.9807852804032304306, 1.000000000000000000, 0.9807852804032304306, 1.000000000000000000, 0.9807852804032304306, 1.000000000000000000, 0.9807852804032304306, 1.000000000000000000, 0.9807852804032304306, 1.000000000000000000, 0.9807852804032304306, 1.000000000000000000, 0.9807852804032304306, 1.000000000000000000, 0.9807852804032304306, 1.000000000000000000, 0.9807852804032304306, 1.000000000000000000, 0.9807852804032304306, 1.000000000000000000, 0.9807852804032304306, 1.000000000000000000, 0.9807852804032304306, 1.000000000000000000, 0.9807852804032304306, 1.000000000000000000, 0.9935442612835747589, 0.9914265054520787768, 0.9914265054520787768, 0.9914265054520787768),
 ( 1.000000000000000000, 0.9807852804032304306, 1.000000000000000000, 0.9807852804032304306, 1.000000000000000000, 0.9807852804032304306, 1.000000000000000000, 0.9807852804032304306, 1.000000000000000000, 0.9807852804032304306, 1.000000000000000000, 0.9807852804032304306, 1.000000000000000000, 0.9807852804032304306, 1.000000000000000000, 0.9807852804032304306, 1.000000000000000000, 0.9807852804032304306, 1.000000000000000000, 0.9807852804032304306, 1.000000000000000000, 0.9807852804032304306, 1.000000000000000000, 0.9807852804032304306, 1.000000000000000000, 0.9807852804032304306, 1.000000000000000000, 0.9807852804032304306, 1.000000000000000000, 0.9807852804032304306, 1.000000000000000000, 0.9807852804032304306, 1.000000000000000000, 0.9807852804032304306, 1.000000000000000000, 0.9807852804032304306, 1.000000000000000000, 0.9807852804032304306, 1.000000000000000000, 0.9807852804032304306, 1.000000000000000000, 0.9807852804032304306, 1.000000000000000000, 0.9807852804032304306, 1.000000000000000000, 0.9807852804032304306, 1.000000000000000000, 0.9807852804032304306, 1.000000000000000000, 0.9807852804032304306, 1.000000000000000000, 0.9807852804032304306, 1.000000000000000000, 0.9807852804032304306, 1.000000000000000000, 0.9807852804032304306, 1.000000000000000000, 0.9807852804032304306, 1.000000000000000000, 0.9807852804032304306, 1.000000000000000000, 0.9807852804032304306, 1.000000000000000000, 0.9807852804032304306, 1.000000000000000000, 0.9807852804032304306, 1.000000000000000000, 0.9807852804032304306, 1.000000000000000000, 0.9807852804032304306, 1.000000000000000000, 0.9807852804032304306, 1.000000000000000000, 0.9807852804032304306, 1.000000000000000000, 0.9807852804032304306, 1.000000000000000000, 0.9807852804032304306, 1.000000000000000000, 0.9807852804032304306, 1.000000000000000000, 0.9807852804032304306, 1.000000000000000000, 0.9807852804032304306, 1.000000000000000000, 0.9807852804032304306, 1.000000000000000000, 0.9807852804032304306, 1.000000000000000000, 0.9807852804032304306, 1.000000000000000000, 0.9807852804032304306, 1.000000000000000000, 0.9807852804032304306, 1.000000000000000000, 0.9807852804032304306, 1.000000000000000000, 0.9807852804032304306, 1.000000000000000000, 0.9807852804032304306, 1.000000000000000000, 0.9807852804032304306, 1.000000000000000000, 0.9807852804032304306, 1.000000000000000000, 0.9807852804032304306, 1.000000000000000000, 0.9807852804032304306, 1.000000000000000000, 0.9807852804032304306, 1.000000000000000000, 0.9807852804032304306, 1.000000000000000000, 0.9807852804032304306, 1.000000000000000000, 0.9807852804032304306, 1.000000000000000000, 0.9807852804032304306, 1.000000000000000000, 0.9807852804032304306, 1.000000000000000000, 0.9807852804032304306, 1.000000000000000000, 0.9807852804032304306, 1.000000000000000000, 0.9807852804032304306, 1.000000000000000000, 0.9807852804032304306, 1.000000000000000000, 0.9807852804032304306, 1.000000000000000000, 0.9807852804032304306, 1.000000000000000000, 0.9807852804032304306, 1.000000000000000000, 0.9807852804032304306, 1.000000000000000000, 0.9807852804032304306, 1.000000000000000000, 0.9807852804032304306, 1.000000000000000000, 0.9807852804032304306, 1.000000000000000000, 0.9807852804032304306, 1.000000000000000000, 0.9807852804032304306, 1.000000000000000000, 0.9807852804032304306, 1.000000000000000000, 0.9807852804032304306, 1.000000000000000000, 0.9807852804032304306, 1.000000000000000000, 0.9807852804032304306, 1.000000000000000000, 0.9807852804032304306, 1.000000000000000000, 0.9807852804032304306, 1.000000000000000000, 0.9807852804032304306, 1.000000000000000000, 0.9807852804032304306, 1.000000000000000000, 0.9807852804032304306, 1.000000000000000000, 0.9807852804032304306, 1.000000000000000000, 0.9807852804032304306, 1.000000000000000000, 0.9807852804032304306, 1.000000000000000000, 0.9807852804032304306, 1.000000000000000000, 0.9807852804032304306, 1.000000000000000000, 0.9807852804032304306, 1.000000000000000000, 0.9807852804032304306, 1.000000000000000000, 0.9807852804032304306, 1.000000000000000000, 0.9807852804032304306, 1.000000000000000000, 0.9807852804032304306, 1.000000000000000000, 0.9807852804032304306, 1.000000000000000000, 0.9807852804032304306, 1.000000000000000000, 0.9807852804032304306, 1.000000000000000000, 0.9807852804032304306, 1.000000000000000000, 0.9807852804032304306, 1.000000000000000000, 0.9807852804032304306, 1.000000000000000000, 0.9807852804032304306, 1.000000000000000000, 0.9807852804032304306, 1.000000000000000000, 0.9807852804032304306, 1.000000000000000000, 0.9807852804032304306, 1.000000000000000000, 0.9807852804032304306, 1.000000000000000000, 0.9807852804032304306, 1.000000000000000000, 0.9807852804032304306, 1.000000000000000000, 0.9807852804032304306, 1.000000000000000000, 0.9807852804032304306, 1.000000000000000000, 0.9807852804032304306, 1.000000000000000000, 0.9807852804032304306, 1.000000000000000000, 0.9807852804032304306, 1.000000000000000000, 0.9807852804032304306, 1.000000000000000000, 0.9807852804032304306, 1.000000000000000000, 0.9807852804032304306, 1.000000000000000000, 0.9807852804032304306, 1.000000000000000000, 0.9807852804032304306, 1.000000000000000000, 0.9807852804032304306, 1.000000000000000000, 0.9807852804032304306, 1.000000000000000000, 0.9807852804032304306, 1.000000000000000000, 0.9807852804032304306, 1.000000000000000000, 0.9807852804032304306, 1.000000000000000000, 0.9807852804032304306, 1.000000000000000000, 0.9807852804032304306, 1.000000000000000000, 0.9807852804032304306, 1.000000000000000000, 0.9807852804032304306, 1.000000000000000000, 0.9807852804032304306, 1.000000000000000000, 0.9807852804032304306, 1.000000000000000000, 0.9807852804032304306, 1.000000000000000000, 0.9807852804032304306, 1.000000000000000000, 0.9807852804032304306, 1.000000000000000000, 0.9807852804032304306, 1.000000000000000000, 0.9807852804032304306, 1.000000000000000000, 0.9807852804032304306, 1.000000000000000000, 0.9807852804032304306, 1.000000000000000000, 0.9807852804032304306, 1.000000000000000000, 0.9807852804032304306, 1.000000000000000000, 0.9807852804032304306, 1.000000000000000000, 0.9807852804032304306, 1.000000000000000000, 0.9807852804032304306, 1.000000000000000000, 0.9807852804032304306, 1.000000000000000000, 0.9807852804032304306, 1.000000000000000000, 0.9807852804032304306, 1.000000000000000000, 0.9807852804032304306, 1.000000000000000000, 0.9807852804032304306, 1.000000000000000000, 0.9807852804032304306, 1.000000000000000000, 0.9807852804032304306, 1.000000000000000000, 0.9807852804032304306, 1.000000000000000000, 0.9807852804032304306, 1.000000000000000000, 0.9807852804032304306, 1.000000000000000000, 0.9807852804032304306, 1.000000000000000000, 0.9807852804032304306, 1.000000000000000000, 0.9807852804032304306, 1.000000000000000000, 0.9807852804032304306, 1.000000000000000000, 0.9807852804032304306, 1.000000000000000000, 0.9807852804032304306, 1.000000000000000000, 0.9807852804032304306, 1.000000000000000000, 0.9807852804032304306, 1.000000000000000000, 0.9807852804032304306, 1.000000000000000000, 0.9807852804032304306, 1.000000000000000000, 0.9807852804032304306, 1.000000000000000000, 0.9807852804032304306, 1.000000000000000000, 0.9807852804032304306, 1.000000000000000000, 0.9807852804032304306, 1.000000000000000000, 0.9807852804032304306, 1.000000000000000000, 0.9807852804032304306, 1.000000000000000000, 0.9807852804032304306, 1.000000000000000000, 0.9807852804032304306, 1.000000000000000000, 0.9807852804032304306, 1.000000000000000000, 0.9807852804032304306, 1.000000000000000000, 0.9807852804032304306, 1.000000000000000000, 0.9807852804032304306, 1.000000000000000000, 0.9807852804032304306, 1.000000000000000000, 0.9807852804032304306, 1.000000000000000000, 0.9807852804032304306, 1.000000000000000000, 0.9807852804032304306, 1.000000000000000000, 0.9807852804032304306, 1.000000000000000000, 0.9807852804032304306, 1.000000000000000000, 0.9807852804032304306, 1.000000000000000000, 0.9807852804032304306, 1.000000000000000000, 0.9807852804032304306, 1.000000000000000000, 0.9807852804032304306, 1.000000000000000000, 0.9807852804032304306, 1.000000000000000000, 0.9807852804032304306, 1.000000000000000000, 0.9807852804032304306, 1.000000000000000000, 0.9807852804032304306, 1.000000000000000000, 0.9807852804032304306, 1.000000000000000000, 0.9807852804032304306, 1.000000000000000000, 0.9807852804032304306, 1.000000000000000000, 0.9807852804032304306, 1.000000000000000000, 0.9807852804032304306, 1.000000000000000000, 0.9807852804032304306, 1.000000000000000000, 0.9807852804032304306, 1.000000000000000000, 0.9807852804032304306, 1.000000000000000000, 0.9807852804032304306, 1.000000000000000000, 0.9807852804032304306, 1.000000000000000000, 0.9807852804032304306, 1.000000000000000000, 0.9807852804032304306, 1.000000000000000000, 0.9807852804032304306, 1.000000000000000000, 0.9807852804032304306, 1.000000000000000000, 0.9807852804032304306, 1.000000000000000000, 0.9807852804032304306, 1.000000000000000000, 0.9807852804032304306, 1.000000000000000000, 0.9807852804032304306, 1.000000000000000000, 0.9807852804032304306, 1.000000000000000000, 0.9807852804032304306, 1.000000000000000000, 0.9807852804032304306, 1.000000000000000000, 0.9807852804032304306, 1.000000000000000000, 0.9807852804032304306, 1.000000000000000000, 0.9807852804032304306, 1.000000000000000000, 0.9807852804032304306, 1.000000000000000000, 0.9807852804032304306, 1.000000000000000000, 0.9807852804032304306, 1.000000000000000000, 0.9807852804032304306, 1.000000000000000000, 0.9807852804032304306, 1.000000000000000000, 0.9807852804032304306, 1.000000000000000000, 0.9807852804032304306, 1.000000000000000000, 0.9807852804032304306, 1.000000000000000000, 0.9807852804032304306, 1.000000000000000000, 0.9807852804032304306, 1.000000000000000000, 0.9807852804032304306, 1.000000000000000000, 0.9807852804032304306, 1.000000000000000000, 0.9807852804032304306, 1.000000000000000000, 0.9807852804032304306, 1.000000000000000000, 0.9807852804032304306, 1.000000000000000000, 0.9807852804032304306, 1.000000000000000000, 0.9807852804032304306, 1.000000000000000000, 0.9807852804032304306, 1.000000000000000000, 0.9807852804032304306, 1.000000000000000000, 0.9807852804032304306, 1.000000000000000000, 0.9807852804032304306, 1.000000000000000000, 0.9807852804032304306, 1.000000000000000000, 0.9807852804032304306, 1.000000000000000000, 0.9807852804032304306, 1.000000000000000000, 0.9807852804032304306, 1.000000000000000000, 0.9807852804032304306, 1.000000000000000000, 0.9807852804032304306, 1.000000000000000000, 0.9807852804032304306, 1.000000000000000000, 0.9807852804032304306, 1.000000000000000000, 0.9807852804032304306, 1.000000000000000000, 0.9807852804032304306, 1.000000000000000000, 0.9807852804032304306, 1.000000000000000000, 0.9807852804032304306, 1.000000000000000000, 0.9807852804032304306, 1.000000000000000000, 0.9807852804032304306, 1.000000000000000000, 0.9807852804032304306, 1.000000000000000000, 0.9807852804032304306, 1.000000000000000000, 0.9807852804032304306, 1.000000000000000000, 0.9807852804032304306, 1.000000000000000000, 0.9807852804032304306, 1.000000000000000000, 0.9807852804032304306, 1.000000000000000000, 0.9807852804032304306, 1.000000000000000000, 0.9807852804032304306, 1.000000000000000000, 0.9807852804032304306, 1.000000000000000000, 0.9807852804032304306, 1.000000000000000000, 0.9807852804032304306, 1.000000000000000000, 0.9807852804032304306, 1.000000000000000000, 0.9807852804032304306, 1.000000000000000000, 0.9807852804032304306, 1.000000000000000000, 0.9807852804032304306, 1.000000000000000000, 0.9807852804032304306, 1.000000000000000000, 0.9807852804032304306, 1.000000000000000000, 0.9807852804032304306, 1.000000000000000000, 0.9807852804032304306, 1.000000000000000000, 0.9807852804032304306, 1.000000000000000000, 0.9807852804032304306, 1.000000000000000000, 0.9807852804032304306, 1.000000000000000000, 0.9807852804032304306, 1.000000000000000000, 0.9807852804032304306, 1.000000000000000000, 0.9807852804032304306, 1.000000000000000000, 0.9807852804032304306, 1.000000000000000000, 0.9807852804032304306, 1.000000000000000000, 0.9807852804032304306, 1.000000000000000000, 0.9807852804032304306, 1.000000000000000000, 0.9807852804032304306, 1.000000000000000000, 0.9807852804032304306, 1.000000000000000000, 0.9807852804032304306, 1.000000000000000000, 0.9807852804032304306, 1.000000000000000000, 0.9807852804032304306, 1.000000000000000000, 0.9807852804032304306, 1.000000000000000000, 0.9807852804032304306, 1.000000000000000000, 0.9807852804032304306, 1.000000000000000000, 0.9807852804032304306, 1.000000000000000000, 0.9807852804032304306, 1.000000000000000000, 0.9807852804032304306, 1.000000000000000000, 0.9807852804032304306, 1.000000000000000000, 0.9807852804032304306, 1.000000000000000000, 0.9807852804032304306, 1.000000000000000000, 0.9807852804032304306, 1.000000000000000000, 0.9807852804032304306, 1.000000000000000000, 0.9807852804032304306, 1.000000000000000000, 0.9807852804032304306, 1.000000000000000000, 0.9807852804032304306, 1.000000000000000000, 0.9807852804032304306, 1.000000000000000000, 0.9807852804032304306, 1.000000000000000000, 0.9807852804032304306, 1.000000000000000000, 0.9807852804032304306, 1.000000000000000000, 0.9807852804032304306, 1.000000000000000000, 0.9807852804032304306, 1.000000000000000000, 0.9807852804032304306, 1.000000000000000000, 0.9807852804032304306, 1.000000000000000000, 0.9807852804032304306, 1.000000000000000000, 0.9807852804032304306, 1.000000000000000000, 0.9807852804032304306, 1.000000000000000000, 0.9807852804032304306, 1.000000000000000000, 0.9807852804032304306, 1.000000000000000000, 0.9807852804032304306, 1.000000000000000000, 0.9807852804032304306, 1.000000000000000000, 0.9807852804032304306, 1.000000000000000000, 0.9807852804032304306, 1.000000000000000000, 0.9807852804032304306, 1.000000000000000000, 0.9807852804032304306, 1.000000000000000000, 0.9807852804032304306, 1.000000000000000000, 0.9807852804032304306, 1.000000000000000000, 0.9807852804032304306, 1.000000000000000000, 0.9807852804032304306, 1.000000000000000000, 0.9807852804032304306, 1.000000000000000000, 0.9807852804032304306, 1.000000000000000000, 0.9807852804032304306, 1.000000000000000000, 0.9807852804032304306, 1.000000000000000000, 0.9807852804032304306, 1.000000000000000000, 0.9807852804032304306, 1.000000000000000000, 0.9807852804032304306, 1.000000000000000000, 0.9807852804032304306, 1.000000000000000000, 0.9807852804032304306, 1.000000000000000000, 0.9807852804032304306, 1.000000000000000000, 0.9807852804032304306, 1.000000000000000000, 0.9807852804032304306, 1.000000000000000000, 0.9807852804032304306, 1.000000000000000000, 0.9807852804032304306, 1.000000000000000000, 0.9807852804032304306, 1.000000000000000000, 0.9807852804032304306, 1.000000000000000000, 0.9807852804032304306, 1.000000000000000000, 0.9807852804032304306, 1.000000000000000000, 0.9807852804032304306, 1.000000000000000000, 0.9807852804032304306, 1.000000000000000000, 0.9807852804032304306, 1.000000000000000000, 0.9807852804032304306, 1.000000000000000000, 0.9807852804032304306, 1.000000000000000000, 0.9807852804032304306, 1.000000000000000000, 0.9807852804032304306, 1.000000000000000000, 0.9807852804032304306, 1.000000000000000000, 0.9807852804032304306, 1.000000000000000000, 0.9807852804032304306, 1.000000000000000000, 0.9807852804032304306, 1.000000000000000000, 0.9807852804032304306, 1.000000000000000000, 0.9807852804032304306, 1.000000000000000000, 0.9807852804032304306, 1.000000000000000000, 0.9807852804032304306, 1.000000000000000000, 0.9807852804032304306, 1.000000000000000000, 0.9807852804032304306, 1.000000000000000000, 0.9807852804032304306, 1.000000000000000000, 0.9807852804032304306, 1.000000000000000000, 0.9807852804032304306, 1.000000000000000000, 0.9807852804032304306, 1.000000000000000000, 0.9807852804032304306, 1.000000000000000000, 0.9807852804032304306, 1.000000000000000000, 0.9807852804032304306, 1.000000000000000000, 0.9807852804032304306, 1.000000000000000000, 0.9807852804032304306, 1.000000000000000000, 0.9807852804032304306, 1.000000000000000000, 0.9807852804032304306, 1.000000000000000000, 0.9807852804032304306, 1.000000000000000000, 0.9807852804032304306, 1.000000000000000000, 0.9807852804032304306, 1.000000000000000000, 0.9807852804032304306, 1.000000000000000000, 0.9807852804032304306, 1.000000000000000000, 0.9807852804032304306, 1.000000000000000000, 0.9807852804032304306, 1.000000000000000000, 0.9807852804032304306, 1.000000000000000000, 0.9807852804032304306, 1.000000000000000000, 0.9807852804032304306, 1.000000000000000000, 0.9807852804032304306, 1.000000000000000000, 0.9807852804032304306, 1.000000000000000000, 0.9807852804032304306, 1.000000000000000000, 0.9807852804032304306, 1.000000000000000000, 0.9807852804032304306, 1.000000000000000000, 0.9807852804032304306, 1.000000000000000000, 0.9807852804032304306, 1.000000000000000000, 0.9807852804032304306, 1.000000000000000000, 0.9807852804032304306, 1.000000000000000000, 0.9807852804032304306, 1.000000000000000000, 0.9807852804032304306, 1.000000000000000000, 0.9807852804032304306, 1.000000000000000000, 0.9807852804032304306, 1.000000000000000000, 0.9807852804032304306, 1.000000000000000000, 0.9807852804032304306, 1.000000000000000000, 0.9807852804032304306, 1.000000000000000000, 0.9807852804032304306, 1.000000000000000000, 0.9807852804032304306, 1.000000000000000000, 0.9807852804032304306, 1.000000000000000000, 0.9807852804032304306, 1.000000000000000000, 0.9807852804032304306, 1.000000000000000000, 0.9807852804032304306, 1.000000000000000000, 0.9807852804032304306, 1.000000000000000000, 0.9807852804032304306, 1.000000000000000000, 0.9807852804032304306, 1.000000000000000000, 0.9807852804032304306, 1.000000000000000000, 0.9807852804032304306, 1.000000000000000000, 0.9807852804032304306, 1.000000000000000000, 0.9807852804032304306, 1.000000000000000000, 0.9807852804032304306, 1.000000000000000000, 0.9807852804032304306, 1.000000000000000000, 0.9807852804032304306, 1.000000000000000000, 0.9807852804032304306, 1.000000000000000000, 0.9807852804032304306, 1.000000000000000000, 0.9807852804032304306, 1.000000000000000000, 0.9807852804032304306, 1.000000000000000000, 0.9807852804032304306, 1.000000000000000000, 0.9807852804032304306, 1.000000000000000000, 0.9807852804032304306, 1.000000000000000000, 0.9807852804032304306, 1.000000000000000000, 0.9807852804032304306, 1.000000000000000000, 0.9807852804032304306, 1.000000000000000000, 0.9807852804032304306, 1.000000000000000000, 0.9807852804032304306, 1.000000000000000000, 0.9807852804032304306, 1.000000000000000000, 0.9807852804032304306, 1.000000000000000000, 0.9807852804032304306, 1.000000000000000000, 0.9807852804032304306, 1.000000000000000000, 0.9807852804032304306, 1.000000000000000000, 0.9807852804032304306, 1.000000000000000000, 0.9807852804032304306, 1.000000000000000000, 0.9807852804032304306, 1.000000000000000000, 0.9807852804032304306, 1.000000000000000000, 0.9807852804032304306, 1.000000000000000000, 0.9807852804032304306, 1.000000000000000000, 0.9807852804032304306, 1.000000000000000000, 0.9807852804032304306, 1.000000000000000000, 0.9807852804032304306, 1.000000000000000000, 0.9807852804032304306, 1.000000000000000000, 0.9807852804032304306, 1.000000000000000000, 0.9807852804032304306, 1.000000000000000000, 0.9807852804032304306, 1.000000000000000000, 0.9807852804032304306, 1.000000000000000000, 0.9807852804032304306, 1.000000000000000000, 0.9807852804032304306, 1.000000000000000000, 0.9807852804032304306, 1.000000000000000000, 0.9807852804032304306, 1.000000000000000000, 0.9807852804032304306, 1.000000000000000000, 0.9807852804032304306, 1.000000000000000000, 0.9807852804032304306, 1.000000000000000000, 0.9807852804032304306, 1.000000000000000000, 0.9807852804032304306, 1.000000000000000000, 0.9807852804032304306, 1.000000000000000000, 0.9807852804032304306, 1.000000000000000000, 0.9807852804032304306, 1.000000000000000000, 0.9807852804032304306, 1.000000000000000000, 0.9807852804032304306, 1.000000000000000000, 0.9807852804032304306, 1.000000000000000000, 0.9807852804032304306, 1.000000000000000000, 0.9807852804032304306, 1.000000000000000000, 0.9807852804032304306, 1.000000000000000000, 0.9807852804032304306, 1.000000000000000000, 0.9807852804032304306, 1.000000000000000000, 0.9807852804032304306, 1.000000000000000000, 0.9807852804032304306, 1.000000000000000000, 0.9807852804032304306, 1.000000000000000000, 0.9807852804032304306, 1.000000000000000000, 0.9807852804032304306, 1.000000000000000000, 0.9807852804032304306, 1.000000000000000000, 0.9807852804032304306, 1.000000000000000000, 0.9807852804032304306, 1.000000000000000000, 0.9807852804032304306, 1.000000000000000000, 0.9807852804032304306, 1.000000000000000000, 0.9807852804032304306, 1.000000000000000000, 0.9807852804032304306, 1.000000000000000000, 0.9807852804032304306, 1.000000000000000000, 0.9807852804032304306, 1.000000000000000000, 0.9807852804032304306, 1.000000000000000000, 0.9807852804032304306, 1.000000000000000000, 0.9807852804032304306, 1.000000000000000000, 0.9807852804032304306, 1.000000000000000000, 0.9807852804032304306, 1.000000000000000000, 0.9807852804032304306, 1.000000000000000000, 0.9807852804032304306, 1.000000000000000000, 0.9807852804032304306, 1.000000000000000000, 0.9807852804032304306, 1.000000000000000000, 0.9807852804032304306, 1.000000000000000000, 0.9807852804032304306, 1.000000000000000000, 0.9807852804032304306, 1.000000000000000000, 0.9807852804032304306, 1.000000000000000000, 0.9807852804032304306, 1.000000000000000000, 0.9807852804032304306, 1.000000000000000000, 0.9807852804032304306, 1.000000000000000000, 0.9807852804032304306, 1.000000000000000000, 0.9807852804032304306, 1.000000000000000000, 0.9807852804032304306, 1.000000000000000000, 0.9807852804032304306, 1.000000000000000000, 0.9807852804032304306, 1.000000000000000000, 0.9807852804032304306, 1.000000000000000000, 0.9807852804032304306, 1.000000000000000000, 0.9807852804032304306, 1.000000000000000000, 0.9807852804032304306, 1.000000000000000000, 0.9807852804032304306, 1.000000000000000000, 0.9807852804032304306, 1.000000000000000000, 0.9807852804032304306, 1.000000000000000000, 0.9807852804032304306, 1.000000000000000000, 0.9807852804032304306, 1.000000000000000000, 0.9807852804032304306, 1.000000000000000000, 0.9807852804032304306, 1.000000000000000000, 0.9807852804032304306, 1.000000000000000000, 0.9807852804032304306, 1.000000000000000000, 0.9935442612835747589, 0.9914265054520787768, 0.9914265054520787768, 0.9914265054520787768) ) ) 
 REPRESENTATION_ITEM ( '' )  SURFACE ( )  );
#18662 = CARTESIAN_POINT ( 'NONE',  ( -35.09675569278793716, 267.2448905683720568, 15.47720386886985366 ) ) ;
#18663 = ORIENTED_EDGE ( 'NONE', *, *, #3274, .T. ) ;
#18664 = VECTOR ( 'NONE', #11505, 1000.000000000000000 ) ;
#18665 = DIRECTION ( 'NONE',  ( -1.232945044042657126E-32, 9.855701800883825964E-17, 1.000000000000000000 ) ) ;
#18666 = CARTESIAN_POINT ( 'NONE',  ( -11.93348319268873503, 480.3698905683720568, -2.051577885510841163E-15 ) ) ;
#18667 = PRESENTATION_LAYER_ASSIGNMENT (  '', '', ( #12459 ) ) ;
#18668 = AXIS2_PLACEMENT_3D ( 'NONE', #8088, #18373, #5071 ) ;
#18669 = VERTEX_POINT ( 'NONE', #10812 ) ;
#18670 = DIRECTION ( 'NONE',  ( -1.000000000000000000, 0.000000000000000000, 0.000000000000000000 ) ) ;
#18671 = CARTESIAN_POINT ( 'NONE',  ( -22.27502019258947286, 250.7448905683720000, -15.47720386886985544 ) ) ;
#18672 = EDGE_LOOP ( 'NONE', ( #17150, #14940, #101, #10905 ) ) ;
#18673 = DIRECTION ( 'NONE',  ( 0.000000000000000000, 0.000000000000000000, 1.000000000000000000 ) ) ;
#18674 = EDGE_CURVE ( 'NONE', #7167, #16774, #7455, .T. ) ;
#18675 = CARTESIAN_POINT ( 'NONE',  ( -14.48388495494898898, 271.3073905683721136, -9.489475012073734561 ) ) ;
#18676 = CARTESIAN_POINT ( 'NONE',  ( -36.33955658999052929, 473.8698905765656377, 18.47759065022572500 ) ) ;
#18677 = CARTESIAN_POINT ( 'NONE',  ( -17.35679799567829207, 390.6823905601785327, 16.95518130045146421 ) ) ;
#18678 = CARTESIAN_POINT ( 'NONE',  ( -13.20868407381884602, 239.7448905683720000, 6.410867750099229490 ) ) ;
#18679 = AXIS2_PLACEMENT_3D ( 'NONE', #19116, #10882, #20850 ) ;
#18680 = CARTESIAN_POINT ( 'NONE',  ( -45.43829269268872650, 525.0573905683720568, -3.332260488124726194 ) ) ;
#18681 = CARTESIAN_POINT ( 'NONE',  ( -10.20829729246298712, 376.3698905765656377, 7.653668647301790529 ) ) ;
#18682 = CARTESIAN_POINT ( 'NONE',  ( -28.68588794268869790, 246.3698905683720000, 16.75240474999999307 ) ) ;
#18683 = CARTESIAN_POINT ( 'NONE',  ( -40.53162694259543741, 364.1198905683720000, -11.84573899990672707 ) ) ;
#18684 = CARTESIAN_POINT ( 'NONE',  ( -123.2946569474810019, 10.52886280891152104, -20.57735571454641388 ) ) ;
#18685 = VECTOR ( 'NONE', #16949, 999.9999999999998863 ) ;
#18686 = VECTOR ( 'NONE', #17238, 1000.000000000000000 ) ;
#18687 = EDGE_CURVE ( 'NONE', #19193, #1608, #7913, .T. ) ;
#18688 = CARTESIAN_POINT ( 'NONE',  ( -32.01814843081345430, 396.0573905683720568, 16.75240474999999307 ) ) ;
#18689 = DIRECTION ( 'NONE',  ( -1.000000000000000000, -0.000000000000000000, -0.000000000000000000 ) ) ;
#18690 = CARTESIAN_POINT ( 'NONE',  ( -17.35679799567830628, 413.8073905601785327, -16.95518130045146421 ) ) ;
#18691 = ORIENTED_EDGE ( 'NONE', *, *, #7639, .F. ) ;
#18692 = FACE_OUTER_BOUND ( 'NONE', #14757, .T. ) ;
#18693 = ORIENTED_EDGE ( 'NONE', *, *, #5440, .T. ) ;
#18694 = ORIENTED_EDGE ( 'NONE', *, *, #10365, .F. ) ;
#18695 = CARTESIAN_POINT ( 'NONE',  ( -32.01814843081346851, 517.5573905683720568, 16.75240474999999307 ) ) ;
#18696 = CARTESIAN_POINT ( 'NONE',  ( -24.70764059509554045, 290.0573905601785327, 19.99999999999998934 ) ) ;
#18697 = DIRECTION ( 'NONE',  ( 1.000000000000000000, 0.000000000000000000, 0.000000000000000000 ) ) ;
#18698 = VERTEX_POINT ( 'NONE', #4229 ) ;
#18699 = ADVANCED_FACE ( 'NONE', ( #12768 ), #4437, .F. ) ;
#18700 = CARTESIAN_POINT ( 'NONE',  ( -28.68588794268870856, 327.8698905683720000, 16.75240474999999307 ) ) ;
#18701 = VERTEX_POINT ( 'NONE', #1206 ) ;
#18702 = CARTESIAN_POINT ( 'NONE',  ( -25.35362745456398059, 346.6823905683720568, 16.75240474999998952 ) ) ;
#18703 = CARTESIAN_POINT ( 'NONE',  ( -38.17536295476245556, 372.3073905683721136, -14.20200298773971426 ) ) ;
#18704 = CARTESIAN_POINT ( 'NONE',  ( -10.20829729246297646, 287.6198905765656377, -7.653668647301794969 ) ) ;
#18705 = CARTESIAN_POINT ( 'NONE',  ( 5.700000000000000178, 0.000000000000000000, 0.000000000000000000 ) ) ;
#18706 = CARTESIAN_POINT ( 'NONE',  ( -35.09675569278793716, 271.9948905683720000, -15.47720386886985544 ) ) ;
#18707 = CARTESIAN_POINT ( 'NONE',  ( 91.21585410611801592, 56.85652257517428865, 94.99999999999994316 ) ) ;
#18708 = CARTESIAN_POINT ( 'NONE',  ( -28.68588794268871922, 407.8698905683720568, 16.75240474999999307 ) ) ;
#18709 = CARTESIAN_POINT ( 'NONE',  ( -8.685887942688742314, 573.2448905601785327, 2.449293598294706119E-15 ) ) ;
#18710 = CARTESIAN_POINT ( 'NONE',  ( -47.16347859291444422, 356.6198905601784759, -7.653668647301793193 ) ) ;
#18711 = DIRECTION ( 'NONE',  ( 0.000000000000000000, -0.000000000000000000, 1.000000000000000000 ) ) ;
#18712 = CARTESIAN_POINT ( 'NONE',  ( -42.88789093042843348, 334.4323905683720568, -9.489475012073736337 ) ) ;
#18713 = CARTESIAN_POINT ( 'NONE',  ( -28.68588794268872988, 461.3698905683720000, -16.75240474999999307 ) ) ;
#18714 = ORIENTED_EDGE ( 'NONE', *, *, #18607, .T. ) ;
#18715 = MECHANICAL_DESIGN_GEOMETRIC_PRESENTATION_REPRESENTATION (  '', ( #13555 ), #12516 ) ;
#18716 = CARTESIAN_POINT ( 'NONE',  ( -17.35679799567830983, 463.8073905601784759, -16.95518130045146421 ) ) ;
#18717 = CARTESIAN_POINT ( 'NONE',  ( -19.19641293061497933, 290.4323905683720000, -14.20200298773971603 ) ) ;
#18718 = ORIENTED_EDGE ( 'NONE', *, *, #15494, .T. ) ;
#18719 = ORIENTED_EDGE ( 'NONE', *, *, #8284, .F. ) ;
#18720 = PLANE ( 'NONE',  #13288 ) ;
#18721 = CARTESIAN_POINT ( 'NONE',  ( -48.68588794268870856, 347.2448905601784759, 0.000000000000000000 ) ) ;
#18722 =( BOUNDED_CURVE ( )  B_SPLINE_CURVE ( 2, ( #837, #5572, #16661, #725, #8816, #9027, #7402, #620, #4058, #18259, #17159, #9926, #15651, #3450, #14028, #7295, #3346 ),
 .UNSPECIFIED., .F., .T. ) 
 B_SPLINE_CURVE_WITH_KNOTS ( ( 3, 2, 2, 2, 2, 2, 2, 2, 3 ),
 ( 0.8437500000000002220, 0.8457031250000002220, 0.8476562500000002220, 0.8496093750000002220, 0.8515625000000002220, 0.8535156250000002220, 0.8554687500000002220, 0.8574218750000002220, 0.8593750000000002220 ),
 .UNSPECIFIED. ) 
 CURVE ( )  GEOMETRIC_REPRESENTATION_ITEM ( )  RATIONAL_B_SPLINE_CURVE ( ( 0.9999999999999977796, 0.9807852804032326510, 1.000000000000000000, 0.9807852804032304306, 1.000000000000000000, 0.9807852804032304306, 1.000000000000000000, 0.9807852804032304306, 1.000000000000000000, 0.9807852804032304306, 1.000000000000000000, 0.9807852804032304306, 1.000000000000000000, 0.9807852804032304306, 1.000000000000000000, 0.9807852804032282101, 1.000000000000002220 ) ) 
 REPRESENTATION_ITEM ( '' )  );
#18723 = CARTESIAN_POINT ( 'NONE',  ( -44.16309181155855867, 304.4948905683720568, 6.410867750099241924 ) ) ;
#18724 = CARTESIAN_POINT ( 'NONE',  ( -25.35362745456398414, 378.1823905683721136, 16.75240474999998952 ) ) ;
#18725 = CARTESIAN_POINT ( 'NONE',  ( -10.20829729246298712, 372.8698905601784759, -7.653668647301794969 ) ) ;
#18726 = CARTESIAN_POINT ( 'NONE',  ( -28.68588794268873698, 529.4948905765655809, -19.99999999999999289 ) ) ;
#18727 = CARTESIAN_POINT ( 'NONE',  ( -44.16309181155857289, 404.4948905683720000, 6.410867750099241924 ) ) ;
#18728 = CARTESIAN_POINT ( 'NONE',  ( -38.17536295476244135, 253.8073905683720568, -14.20200298773971426 ) ) ;
#18729 = ADVANCED_FACE ( 'NONE', ( #10699 ), #9298, .F. ) ;
#18730 = AXIS2_PLACEMENT_3D ( 'NONE', #940, #10861, #723 ) ;
#18731 = CARTESIAN_POINT ( 'NONE',  ( -42.88789093042844058, 422.9323905683720000, -9.489475012073734561 ) ) ;
#18732 = ITEM_DEFINED_TRANSFORMATION ( 'NONE', 'NONE', #12473,  #12794 ) ;
#18733 = EDGE_CURVE ( 'NONE', #12668, #18325, #2607, .T. ) ;
#18734 = CARTESIAN_POINT ( 'NONE',  ( -32.66413529028187668, 344.1823905765656377, 19.99999999999999289 ) ) ;
#18735 = DIRECTION ( 'NONE',  ( -1.000000000000000000, 0.000000000000000000, -0.000000000000000000 ) ) ;
#18736 = CARTESIAN_POINT ( 'NONE',  ( -45.43829269268870519, 323.5573905683720000, -3.332260488124726638 ) ) ;
#18737 = CARTESIAN_POINT ( 'NONE',  ( -28.68588794268872988, 482.8698905683720568, -16.75240474999999307 ) ) ;
#18738 = DIRECTION ( 'NONE',  ( 0.000000000000000000, 1.000000000000000000, -0.000000000000000000 ) ) ;
#18739 = CARTESIAN_POINT ( 'NONE',  ( -28.68588794268874054, 573.2448905601785327, 0.000000000000000000 ) ) ;
#18740 = CARTESIAN_POINT ( 'NONE',  ( -36.33955658999050087, 305.3698905601784759, -18.47759065022572855 ) ) ;
#18741 = CARTESIAN_POINT ( 'NONE',  ( -25.35362745456398414, 378.1823905683720568, 16.75240474999998952 ) ) ;
#18742 = CARTESIAN_POINT ( 'NONE',  ( 51.50493485826542184, 160.1716627696692683, -61.61851857202071159 ) ) ;
#18743 = AXIS2_PLACEMENT_3D ( 'NONE', #17704, #10776, #17492 ) ;
#18744 = CARTESIAN_POINT ( 'NONE',  ( -47.16347859291446554, 517.8698905601785327, 7.653668647301805628 ) ) ;
#18745 = CARTESIAN_POINT ( 'NONE',  ( -19.19641293061498644, 350.4323905683720000, -14.20200298773971603 ) ) ;
#18746 = ORIENTED_EDGE ( 'NONE', *, *, #19316, .F. ) ;
#18747 = CARTESIAN_POINT ( 'NONE',  ( -42.88789093042844769, 502.9323905683720000, -9.489475012073736337 ) ) ;
#18748 = ORIENTED_EDGE ( 'NONE', *, *, #14701, .T. ) ;
#18749 = CARTESIAN_POINT ( 'NONE',  ( -36.33955658999051508, 349.1198905601784759, 18.47759065022572500 ) ) ;
#18750 = CARTESIAN_POINT ( 'NONE',  ( -24.70764059509556176, 379.1823905765656377, -19.99999999999999289 ) ) ;
#18751 = CARTESIAN_POINT ( 'NONE',  ( 6.416697501590670427, 172.9933428177121471, 50.00000000000000000 ) ) ;
#18752 = CARTESIAN_POINT ( 'NONE',  ( -48.68588794268870856, 377.2448905601784759, 0.000000000000000000 ) ) ;
#18753 = FACE_OUTER_BOUND ( 'NONE', #3902, .T. ) ;
#18754 = CARTESIAN_POINT ( 'NONE',  ( -32.01814843081346140, 456.0573905683720000, 16.75240474999999307 ) ) ;
#18755 = ORIENTED_EDGE ( 'NONE', *, *, #6268, .F. ) ;
#18756 = CARTESIAN_POINT ( 'NONE',  ( -40.53162694259545162, 495.1198905683720000, 11.84573899990672885 ) ) ;
#18757 = CARTESIAN_POINT ( 'NONE',  ( -48.68588794268872277, 487.2448905601784759, 0.000000000000000000 ) ) ;
#18758 = CIRCLE ( 'NONE', #13950, 175.0000000000000284 ) ;
#18759 = CARTESIAN_POINT ( 'NONE',  ( -8.685887942688726326, 407.3073905765656377, -3.978247347593165895 ) ) ;
#18760 = DIRECTION ( 'NONE',  ( -0.000000000000000000, -0.000000000000000000, -1.000000000000000000 ) ) ;
#18761 = CARTESIAN_POINT ( 'NONE',  ( -48.68588794268870146, 297.2448905601784759, 0.000000000000000000 ) ) ;
#18762 = CARTESIAN_POINT ( 'NONE',  ( -40.01497788969915348, 485.6823905601785327, -16.95518130045146421 ) ) ;
#18763 = FACE_BOUND ( 'NONE', #14571, .T. ) ;
#18764 = DIRECTION ( 'NONE',  ( 0.000000000000000000, -1.000000000000000000, 0.000000000000000000 ) ) ;
#18765 = CARTESIAN_POINT ( 'NONE',  ( -17.35679799567830273, 433.8073905601784759, -16.95518130045146421 ) ) ;
#18766 = CARTESIAN_POINT ( 'NONE',  ( -1.052014920489841021E-15, -5.469921996229796690, 3.525817189091422943 ) ) ;
#18767 = CARTESIAN_POINT ( 'NONE',  ( -40.53162694259543031, 284.1198905683720000, -11.84573899990672707 ) ) ;
#18768 = CARTESIAN_POINT ( 'NONE',  ( -48.68588794268869435, 247.2448905601785043, 0.000000000000000000 ) ) ;
#18769 = CARTESIAN_POINT ( 'NONE',  ( -42.82802356641965957, 363.2448905765656377, 14.14213562373094923 ) ) ;
#18770 = CARTESIAN_POINT ( 'NONE',  ( -38.17536295476246266, 443.8073905683720568, -14.20200298773971426 ) ) ;
#18771 = CARTESIAN_POINT ( 'NONE',  ( -48.68588794268854514, 331.6823905765656377, -3.978247347593583783 ) ) ;
#18772 = CARTESIAN_POINT ( 'NONE',  ( -19.19641293061497578, 261.9323905683720568, -14.20200298773971603 ) ) ;
#18773 = VECTOR ( 'NONE', #13905, 1000.000000000000000 ) ;
#18774 = EDGE_LOOP ( 'NONE', ( #8428, #132, #7709, #13981 ) ) ;
#18775 = CARTESIAN_POINT ( 'NONE',  ( -13.20868407381887444, 489.7448905683720568, 6.410867750099229490 ) ) ;
#18776 = AXIS2_PLACEMENT_3D ( 'NONE', #750, #2469, #7315 ) ;
#18777 = CIRCLE ( 'NONE', #19148, 0.4000000000000001887 ) ;
#18778 = ORIENTED_EDGE ( 'NONE', *, *, #6761, .F. ) ;
#18779 = EDGE_CURVE ( 'NONE', #1584, #16350, #15667, .T. ) ;
#18780 = LINE ( 'NONE', #17176, #11053 ) ;
#18781 = CARTESIAN_POINT ( 'NONE',  ( -14.48388495494898542, 249.8073905683720568, -9.489475012073736337 ) ) ;
#18782 = VERTEX_POINT ( 'NONE', #12662 ) ;
#18783 = CARTESIAN_POINT ( 'NONE',  ( 149.4511408718632879, 610.7448905601785327, -3.512089204514984520 ) ) ;
#18784 = CARTESIAN_POINT ( 'NONE',  ( -14.54375231895778420, 478.2448905765655809, -14.14213562373094746 ) ) ;
#18785 = DIRECTION ( 'NONE',  ( -0.000000000000000000, 1.000000000000000000, -0.000000000000000000 ) ) ;
#18786 = CARTESIAN_POINT ( 'NONE',  ( -24.39804996317073105, 223.9102039777117739, -18.69641520486996100 ) ) ;
#18787 = CARTESIAN_POINT ( 'NONE',  ( -28.68588794268870146, 242.8698905683720568, -16.75240474999999307 ) ) ;
#18788 = CARTESIAN_POINT ( 'NONE',  ( -45.43829269268872650, 515.0573905683720568, -3.332260488124726194 ) ) ;
#18789 = CARTESIAN_POINT ( 'NONE',  ( 0.000000000000000000, 5.629165124598848102, 3.250000000000005329 ) ) ;
#18790 = CARTESIAN_POINT ( 'NONE',  ( -38.17536295476243424, 245.4323905683720000, 14.20200298773971781 ) ) ;
#18791 =( BOUNDED_CURVE ( )  B_SPLINE_CURVE ( 2, ( #17015, #18940, #15612, #8671, #12353, #2197, #16910, #7365, #4017, #19058, #4125, #20254, #8782, #10711, #3913, #15295, #12460 ),
 .UNSPECIFIED., .F., .T. ) 
 B_SPLINE_CURVE_WITH_KNOTS ( ( 3, 2, 2, 2, 2, 2, 2, 2, 3 ),
 ( 0.7500000000000001110, 0.7519531250000001110, 0.7539062500000001110, 0.7558593750000001110, 0.7578125000000001110, 0.7597656250000001110, 0.7617187500000001110, 0.7636718750000001110, 0.7656250000000001110 ),
 .UNSPECIFIED. ) 
 CURVE ( )  GEOMETRIC_REPRESENTATION_ITEM ( )  RATIONAL_B_SPLINE_CURVE ( ( 0.9999999999999988898, 0.9807852804032315408, 1.000000000000000000, 0.9807852804032304306, 1.000000000000000000, 0.9807852804032304306, 1.000000000000000000, 0.9807852804032304306, 1.000000000000000000, 0.9807852804032304306, 1.000000000000000000, 0.9807852804032304306, 1.000000000000000000, 0.9807852804032304306, 1.000000000000000000, 0.9807852804032293204, 1.000000000000001110 ) ) 
 REPRESENTATION_ITEM ( '' )  );
#18792 = AXIS2_PLACEMENT_3D ( 'NONE', #11709, #8455, #18302 ) ;
#18793 = CARTESIAN_POINT ( 'NONE',  ( -40.53162694259543741, 346.6198905683720000, 11.84573899990672885 ) ) ;
#18794 = DIRECTION ( 'NONE',  ( 0.000000000000000000, 0.000000000000000000, 1.000000000000000000 ) ) ;
#18795 = EDGE_CURVE ( 'NONE', #3515, #19311, #2570, .T. ) ;
#18796 = CARTESIAN_POINT ( 'NONE',  ( -32.01814843081345430, 411.6823905683720568, -16.75240474999999307 ) ) ;
#18797 = LINE ( 'NONE', #7433, #1186 ) ;
#18798 = CARTESIAN_POINT ( 'NONE',  ( -14.54375231895776821, 380.9948905601784759, 14.14213562373094568 ) ) ;
#18799 = VERTEX_POINT ( 'NONE', #17737 ) ;
#18800 = CARTESIAN_POINT ( 'NONE',  ( -174.5421710038924061, 600.7448905601785327, 96.70028278950401557 ) ) ;
#18801 = EDGE_LOOP ( 'NONE', ( #7019, #9282, #15286 ) ) ;
#18802 = VERTEX_POINT ( 'NONE', #18927 ) ;
#18803 = CARTESIAN_POINT ( 'NONE',  ( -22.27502019258950128, 512.2448905683720568, -15.47720386886985544 ) ) ;
#18804 = CARTESIAN_POINT ( 'NONE',  ( -43.20801099888741703, 208.4516271390267548, -3.763513762345671143 ) ) ;
#18805 = VERTEX_POINT ( 'NONE', #2929 ) ;
#18806 = CARTESIAN_POINT ( 'NONE',  ( -42.88789093042842637, 306.3073905683720000, 9.489475012073734561 ) ) ;
#18807 = ORIENTED_EDGE ( 'NONE', *, *, #18733, .F. ) ;
#18808 = CARTESIAN_POINT ( 'NONE',  ( -35.09675569278794427, 341.9948905683720000, -15.47720386886985544 ) ) ;
#18809 = CARTESIAN_POINT ( 'NONE',  ( -35.09675569278794427, 351.9948905683720000, -15.47720386886985544 ) ) ;
#18810 = EDGE_CURVE ( 'NONE', #11758, #12017, #12446, .T. ) ;
#18811 = CARTESIAN_POINT ( 'NONE',  ( -24.70764059509554045, 284.8073905765655809, 19.99999999999998934 ) ) ;
#18812 = CARTESIAN_POINT ( 'NONE',  ( -10.20829729246300310, 497.6198905765656377, -7.653668647301794969 ) ) ;
#18813 = CARTESIAN_POINT ( 'NONE',  ( -44.16309181155855157, 254.4948905683720568, 6.410867750099241924 ) ) ;
#18814 = CARTESIAN_POINT ( 'NONE',  ( -45.64106924314016567, 226.3073905601784759, -11.32908994701042538 ) ) ;
#18815 = CARTESIAN_POINT ( 'NONE',  ( -40.53162694259544452, 404.1198905683720000, -11.84573899990672707 ) ) ;
#18816 = CARTESIAN_POINT ( 'NONE',  ( -8.685887942688541585, 332.5573905601783622, -3.978247347592740013 ) ) ;
#18817 = CARTESIAN_POINT ( 'NONE',  ( -24.70764059509556532, 504.8073905765656377, 19.99999999999998934 ) ) ;
#18818 = DIRECTION ( 'NONE',  ( -0.9510565162951536422, -1.133459776540192663E-16, -0.3090169943749472292 ) ) ;
#18819 = ADVANCED_FACE ( 'NONE', ( #18052 ), #13201, .F. ) ;
#18820 = CARTESIAN_POINT ( 'NONE',  ( -38.17536295476244135, 306.9323905683719431, 14.20200298773971781 ) ) ;
#18821 = CARTESIAN_POINT ( 'NONE',  ( -22.27502019258949062, 466.9948905683720000, 15.47720386886985189 ) ) ;
#18822 = ORIENTED_EDGE ( 'NONE', *, *, #8780, .T. ) ;
#18823 = CARTESIAN_POINT ( 'NONE',  ( -8.685887942688735208, 461.9323905601785327, 3.978247347593161010 ) ) ;
#18824 = CARTESIAN_POINT ( 'NONE',  ( -40.53162694259543031, 292.6198905683720000, -11.84573899990672707 ) ) ;
#18825 = EDGE_LOOP ( 'NONE', ( #12345, #3357, #19990, #1720 ) ) ;
#18826 = CARTESIAN_POINT ( 'NONE',  ( 14.09825962131072785, 160.1716627696692683, 49.99999999999999289 ) ) ;
#18827 = ORIENTED_EDGE ( 'NONE', *, *, #5521, .F. ) ;
#18828 = ORIENTED_EDGE ( 'NONE', *, *, #18213, .F. ) ;
#18829 = PLANE ( 'NONE',  #5672 ) ;
#18830 = CARTESIAN_POINT ( 'NONE',  ( -13.20868407381885135, 308.2448905683720000, 6.410867750099229490 ) ) ;
#18831 = CARTESIAN_POINT ( 'NONE',  ( -44.16309181155857289, 374.7448905683720568, -6.410867750099231266 ) ) ;
#18832 = LINE ( 'NONE', #7148, #4855 ) ;
#18833 = CARTESIAN_POINT ( 'NONE',  ( -36.33955658999053639, 523.8698905765655809, 18.47759065022572500 ) ) ;
#18834 = CARTESIAN_POINT ( 'NONE',  ( -40.53162694259544452, 395.1198905683720000, 11.84573899990672885 ) ) ;
#18835 = CARTESIAN_POINT ( 'NONE',  ( -45.43829269268869808, 235.3698905683720284, 0.000000000000000000 ) ) ;
#18836 = CARTESIAN_POINT ( 'NONE',  ( -45.43829269268871940, 424.1823905683721136, 3.332260488124734632 ) ) ;
#18837 = CARTESIAN_POINT ( 'NONE',  ( -11.73070664223724613, 346.0573905765656377, 11.32908994701042005 ) ) ;
#18838 = LINE ( 'NONE', #12255, #7203 ) ;
#18839 = CARTESIAN_POINT ( 'NONE',  ( -42.88789093042842637, 314.8073905683721136, 9.489475012073734561 ) ) ;
#18840 = CARTESIAN_POINT ( 'NONE',  ( -11.93348319268873503, 480.6823905683720000, -3.332260488124732856 ) ) ;
#18841 = CARTESIAN_POINT ( 'NONE',  ( -10.20829729246300488, 516.3698905765656946, 7.653668647301790529 ) ) ;
#18842 = CARTESIAN_POINT ( 'NONE',  ( -43.63022347157595249, 200.3131325479158704, -1.300740588846951651 ) ) ;
#18843 = LINE ( 'NONE', #4032, #9539 ) ;
#18844 = CARTESIAN_POINT ( 'NONE',  ( -45.43829269268871229, 395.0573905683719431, -3.332260488124726194 ) ) ;
#18845 = CARTESIAN_POINT ( 'NONE',  ( -33.84809828339280102, 56.08443449083164012, -120.3299889578561448 ) ) ;
#18846 = EDGE_CURVE ( 'NONE', #19418, #14194, #17837, .T. ) ;
#18847 = SHAPE_REPRESENTATION ( 'Heavy Perimeter Inertia Flywheel Disk', ( #12794 ), #20056 ) ;
#18848 = CARTESIAN_POINT ( 'NONE',  ( -42.82802356641968089, 525.9948905601785327, -14.14213562373094746 ) ) ;
#18849 = CARTESIAN_POINT ( 'NONE',  ( -42.88789093042843348, 344.8073905683719431, 9.489475012073736337 ) ) ;
#18850 = VERTEX_POINT ( 'NONE', #8201 ) ;
#18851 = CARTESIAN_POINT ( 'NONE',  ( -45.43829269268873361, 513.8698905683720568, 0.000000000000000000 ) ) ;
#18852 = ORIENTED_EDGE ( 'NONE', *, *, #15910, .F. ) ;
#18853 = CARTESIAN_POINT ( 'NONE',  ( -44.33485469295106185, 223.9102039777117454, -6.015342892178036749 ) ) ;
#18854 = DIRECTION ( 'NONE',  ( 0.3090169943749475068, 0.000000000000000000, 0.9510565162951535312 ) ) ;
#18855 = CARTESIAN_POINT ( 'NONE',  ( -40.01497788969913216, 290.4323905765656946, -16.95518130045146421 ) ) ;
#18856 = LINE ( 'NONE', #20386, #6226 ) ;
#18857 = CARTESIAN_POINT ( 'NONE',  ( -45.43829269268871940, 463.5573905683720568, -3.332260488124726194 ) ) ;
#18858 = ORIENTED_EDGE ( 'NONE', *, *, #11610, .F. ) ;
#18859 = CARTESIAN_POINT ( 'NONE',  ( -14.48388495494901029, 477.9323905683721136, 9.489475012073731008 ) ) ;
#18860 = CARTESIAN_POINT ( 'NONE',  ( 0.2573354458087815932, 4.368923434677189022, 5.432802636760778014 ) ) ;
#18861 = EDGE_CURVE ( 'NONE', #14411, #19262, #3351, .T. ) ;
#18862 = CARTESIAN_POINT ( 'NONE',  ( -21.03221929538692692, 398.8698905765656377, -18.47759065022572855 ) ) ;
#18863 = CARTESIAN_POINT ( 'NONE',  ( -21.03221929538692336, 475.1198905765656377, 18.47759065022572500 ) ) ;
#18864 = CARTESIAN_POINT ( 'NONE',  ( -8.685887942688735208, 482.2448905601784759, -2.449293598294705724E-15 ) ) ;
#18865 = LINE ( 'NONE', #4056, #2859 ) ;
#18866 = EDGE_CURVE ( 'NONE', #2991, #16878, #7100, .T. ) ;
#18867 = ADVANCED_FACE ( 'NONE', ( #6367 ), #6263, .T. ) ;
#18868 = AXIS2_PLACEMENT_3D ( 'NONE', #11428, #9593, #14486 ) ;
#18869 = DIRECTION ( 'NONE',  ( 0.000000000000000000, -0.8660254037844380415, 0.5000000000000012212 ) ) ;
#18870 = CARTESIAN_POINT ( 'NONE',  ( -8.685887942688708563, 242.2448905601785043, -2.449293598294705724E-15 ) ) ;
#18871 = CARTESIAN_POINT ( 'NONE',  ( -28.68588794268869790, 213.9102039777116602, 0.000000000000000000 ) ) ;
#18872 = CARTESIAN_POINT ( 'NONE',  ( -32.01814843081344009, 277.5573905683720000, 16.75240474999999307 ) ) ;
#18873 = CARTESIAN_POINT ( 'NONE',  ( -45.64106924314017277, 248.1823905601785043, 11.32908994701042715 ) ) ;
#18874 = AXIS2_PLACEMENT_3D ( 'NONE', #12534, #2690, #15890 ) ;
#18875 = CARTESIAN_POINT ( 'NONE',  ( -8.685887942688902186, 366.6823905765656377, 3.978247347593586447 ) ) ;
#18876 = CARTESIAN_POINT ( 'NONE',  ( -11.93348319268872970, 440.0573905683720000, 3.332260488124728415 ) ) ;
#18877 = CARTESIAN_POINT ( 'NONE',  ( -14.54375231895776643, 328.2448905765656377, -14.14213562373094746 ) ) ;
#18878 = CARTESIAN_POINT ( 'NONE',  ( -11.93348319268870839, 260.3698905683720000, -2.051577885510841163E-15 ) ) ;
#18879 = B_SPLINE_CURVE_WITH_KNOTS ( 'NONE', 3,
 ( #20915, #17665, #8123, #4474, #14539, #9441, #7708, #21340 ),
 .UNSPECIFIED., .F., .F.,
 ( 4, 2, 2, 4 ),
 ( 0.003797433802554451947, 0.004743183970586247432, 0.005688934138618042050, 0.007580434474681631285 ),
 .UNSPECIFIED. ) ;
#18880 = EDGE_CURVE ( 'NONE', #5244, #9516, #16234, .T. ) ;
#18881 = ORIENTED_EDGE ( 'NONE', *, *, #13562, .T. ) ;
#18882 = DIRECTION ( 'NONE',  ( -1.191790137725560488E-16, 1.000000000000000000, -0.000000000000000000 ) ) ;
#18883 = VERTEX_POINT ( 'NONE', #11345 ) ;
#18884 = CARTESIAN_POINT ( 'NONE',  ( -28.68588794268872988, 482.8698905683720568, -16.75240474999999307 ) ) ;
#18885 = AXIS2_PLACEMENT_3D ( 'NONE', #4520, #21276, #6029 ) ;
#18886 = EDGE_LOOP ( 'NONE', ( #13985, #2827, #14367, #11876 ) ) ;
#18887 = DIRECTION ( 'NONE',  ( 1.000000000000000000, 0.000000000000000000, 0.000000000000000000 ) ) ;
#18888 = CARTESIAN_POINT ( 'NONE',  ( -19.19641293061497223, 250.4323905683720284, -14.20200298773971603 ) ) ;
#18889 = ORIENTED_EDGE ( 'NONE', *, *, #13069, .T. ) ;
#18890 = CARTESIAN_POINT ( 'NONE',  ( 18.55315245287936321, 130.1716627696692683, 1.734723475976807094E-15 ) ) ;
#18891 = CIRCLE ( 'NONE', #18535, 38.00000000000000000 ) ;
#18892 = CARTESIAN_POINT ( 'NONE',  ( -36.33955658999052218, 460.1198905765655809, -18.47759065022572855 ) ) ;
#18893 = DIRECTION ( 'NONE',  ( 0.000000000000000000, -0.000000000000000000, 1.000000000000000000 ) ) ;
#18894 = CARTESIAN_POINT ( 'NONE',  ( -45.64106924314019409, 456.3073905601785327, -11.32908994701042538 ) ) ;
#18895 = DIRECTION ( 'NONE',  ( -0.000000000000000000, 1.000000000000000000, -0.000000000000000000 ) ) ;
#18896 = CARTESIAN_POINT ( 'NONE',  ( -25.35362745456399836, 518.1823905683720568, 16.75240474999998952 ) ) ;
#18897 = FILL_AREA_STYLE ('',( #15887 ) ) ;
#18898 = CARTESIAN_POINT ( 'NONE',  ( -45.43829269268869098, 254.1823905683719715, 3.332260488124734632 ) ) ;
#18899 = CARTESIAN_POINT ( 'NONE',  ( -28.68588794268871212, 332.8698905683720000, -16.75240474999999307 ) ) ;
#18900 = VECTOR ( 'NONE', #14715, 1000.000000000000000 ) ;
#18901 = CARTESIAN_POINT ( 'NONE',  ( -8.685887942688868435, 471.9323905601783622, 3.978247347593479866 ) ) ;
#18902 = CARTESIAN_POINT ( 'NONE',  ( -14.54375231895776643, 360.9948905601784759, 14.14213562373094568 ) ) ;
#18903 = AXIS2_PLACEMENT_3D ( 'NONE', #8443, #20137, #358 ) ;
#18904 = CARTESIAN_POINT ( 'NONE',  ( -42.88789093042844058, 392.9323905683720568, -9.489475012073736337 ) ) ;
#18905 = CARTESIAN_POINT ( 'NONE',  ( -45.43829269268873361, 535.0573905683719431, -3.332260488124726638 ) ) ;
#18906 = CARTESIAN_POINT ( 'NONE',  ( -21.03221929538691271, 390.3698905601785327, 18.47759065022572500 ) ) ;
#18907 = CARTESIAN_POINT ( 'NONE',  ( -31.26501780185373391, 205.1437886375728965, 0.000000000000000000 ) ) ;
#18908 = VERTEX_POINT ( 'NONE', #1411 ) ;
#18909 = ORIENTED_EDGE ( 'NONE', *, *, #10014, .F. ) ;
#18910 = CARTESIAN_POINT ( 'NONE',  ( -13.20868407381887799, 510.9948905683721136, -6.410867750099233042 ) ) ;
#18911 = CARTESIAN_POINT ( 'NONE',  ( -14.54375231895775933, 295.7448905765656377, 14.14213562373094568 ) ) ;
#18912 = ORIENTED_EDGE ( 'NONE', *, *, #5721, .T. ) ;
#18913 = CARTESIAN_POINT ( 'NONE',  ( -19.19641293061497223, 308.8073905683721136, 14.20200298773971426 ) ) ;
#18914 = ORIENTED_EDGE ( 'NONE', *, *, #19782, .T. ) ;
#18915 = CARTESIAN_POINT ( 'NONE',  ( -19.19641293061497933, 337.3073905683720568, 14.20200298773971426 ) ) ;
#18916 = CARTESIAN_POINT ( 'NONE',  ( -42.88789093042843348, 342.9323905683721136, -9.489475012073734561 ) ) ;
#18917 = EDGE_CURVE ( 'NONE', #984, #2721, #14507, .T. ) ;
#18918 = CARTESIAN_POINT ( 'NONE',  ( -48.68588794268870146, 282.3073905765656377, 3.978247347593168115 ) ) ;
#18919 = LINE ( 'NONE', #7667, #13806 ) ;
#18920 = CARTESIAN_POINT ( 'NONE',  ( -42.88789093042841927, 254.8073905683720284, 9.489475012073734561 ) ) ;
#18921 = CARTESIAN_POINT ( 'NONE',  ( -42.88696169552117965, 203.8418613323789543, 4.830328443944832628 ) ) ;
#18922 = CARTESIAN_POINT ( 'NONE',  ( -22.27502019258947996, 398.4948905683720000, 15.47720386886985189 ) ) ;
#18923 = CARTESIAN_POINT ( 'NONE',  ( 45.67500000000000426, 0.000000000000000000, 0.000000000000000000 ) ) ;
#18924 = CARTESIAN_POINT ( 'NONE',  ( -8.685887942689081598, 506.6823905765655240, 3.978247347593985683 ) ) ;
#18925 = PRODUCT_RELATED_PRODUCT_CATEGORY ( 'part', '', ( #7491 ) ) ;
#18926 = UNCERTAINTY_MEASURE_WITH_UNIT (LENGTH_MEASURE( 1.000000000000000082E-05 ), #12998, 'distance_accuracy_value', 'NONE');
#18927 = CARTESIAN_POINT ( 'NONE',  ( -8.685887942688713892, 286.9948905765656377, -2.449293598294705724E-15 ) ) ;
#18928 = CARTESIAN_POINT ( 'NONE',  ( -42.88789093042844769, 462.9323905683720568, -9.489475012073736337 ) ) ;
#18929 = ORIENTED_EDGE ( 'NONE', *, *, #21136, .T. ) ;
#18930 = CARTESIAN_POINT ( 'NONE',  ( -32.66413529028189089, 455.0573905601785327, -19.99999999999999289 ) ) ;
#18931 = EDGE_CURVE ( 'NONE', #10415, #3879, #1851, .T. ) ;
#18932 = ORIENTED_EDGE ( 'NONE', *, *, #20130, .T. ) ;
#18933 = CARTESIAN_POINT ( 'NONE',  ( -48.68588794268870856, 337.2448905601784759, 0.000000000000000000 ) ) ;
#18934 = EDGE_LOOP ( 'NONE', ( #12647, #14651, #9144 ) ) ;
#18935 = ORIENTED_EDGE ( 'NONE', *, *, #9217, .F. ) ;
#18936 = DIRECTION ( 'NONE',  ( 0.000000000000000000, 0.000000000000000000, -1.000000000000000000 ) ) ;
#18937 = CARTESIAN_POINT ( 'NONE',  ( -40.01497788969913216, 348.8073905601784190, 16.95518130045146776 ) ) ;
#18938 = CARTESIAN_POINT ( 'NONE',  ( -11.93348319268871727, 309.1823905683719431, -3.332260488124732856 ) ) ;
#18939 = CARTESIAN_POINT ( 'NONE',  ( -13.20868407381885845, 359.7448905683720568, 6.410867750099229490 ) ) ;
#18940 = CARTESIAN_POINT ( 'NONE',  ( -48.68588794268860909, 296.9323905601784759, -3.978247347593371508 ) ) ;
#18941 = CARTESIAN_POINT ( 'NONE',  ( -8.685887942688742314, 526.9948905765655809, -2.449293598294705724E-15 ) ) ;
#18942 = CARTESIAN_POINT ( 'NONE',  ( -38.17536295476246266, 412.3073905683720000, -14.20200298773971426 ) ) ;
#18943 = CARTESIAN_POINT ( 'NONE',  ( -25.35362745456397704, 232.5573905683720568, -16.75240474999999307 ) ) ;
#18944 = CARTESIAN_POINT ( 'NONE',  ( -13.20868407381886378, 408.2448905683720568, 6.410867750099229490 ) ) ;
#18945 = CONTEXT_DEPENDENT_SHAPE_REPRESENTATION ( #7078, #12696 ) ;
#18946 = AXIS2_PLACEMENT_3D ( 'NONE', #17649, #7894, #21107 ) ;
#18947 = EDGE_CURVE ( 'NONE', #8426, #16109, #12877, .T. ) ;
#18948 = CARTESIAN_POINT ( 'NONE',  ( -10.20829729246298356, 346.3698905765655809, 7.653668647301790529 ) ) ;
#18949 = EDGE_CURVE ( 'NONE', #18299, #12191, #14826, .T. ) ;
#18950 = CARTESIAN_POINT ( 'NONE',  ( -48.68588794268870146, 327.2448905601785327, 0.000000000000000000 ) ) ;
#18951 = CARTESIAN_POINT ( 'NONE',  ( -25.35362745456397349, 296.6823905683720568, 16.75240474999998952 ) ) ;
#18952 = CARTESIAN_POINT ( 'NONE',  ( -14.48388495494900852, 459.4323905683720568, 9.489475012073732785 ) ) ;
#18953 = LINE ( 'NONE', #13334, #5090 ) ;
#18954 = CARTESIAN_POINT ( 'NONE',  ( -42.82802356641966668, 204.8142847187656059, -5.000000000000003553 ) ) ;
#18955 = CARTESIAN_POINT ( 'NONE',  ( -11.93348319268872260, 370.3698905683720568, -2.051577885510841163E-15 ) ) ;
#18956 = CARTESIAN_POINT ( 'NONE',  ( -28.68588794268875475, 600.7448905601785327, 0.000000000000000000 ) ) ;
#18957 = CARTESIAN_POINT ( 'NONE',  ( -42.82802356641968089, 515.9948905601785327, -14.14213562373094746 ) ) ;
#18958 = CARTESIAN_POINT ( 'NONE',  ( -25.35362745456397704, 336.6823905683720568, 16.75240474999998952 ) ) ;
#18959 = AXIS2_PLACEMENT_3D ( 'NONE', #275, #18735, #13458 ) ;
#18960 = EDGE_CURVE ( 'NONE', #15977, #3882, #16007, .T. ) ;
#18961 = VERTEX_POINT ( 'NONE', #16092 ) ;
#18962 = CARTESIAN_POINT ( 'NONE',  ( -25.35362745456399836, 496.6823905683721136, 16.75240474999998952 ) ) ;
#18963 = ORIENTED_EDGE ( 'NONE', *, *, #19394, .F. ) ;
#18964 = CARTESIAN_POINT ( 'NONE',  ( -10.20829729246298356, 351.6198905601784759, 7.653668647301790529 ) ) ;
#18965 = LINE ( 'NONE', #5450, #1734 ) ;
#18966 = CARTESIAN_POINT ( 'NONE',  ( -24.70764059509554755, 314.8073905765655809, 19.99999999999998934 ) ) ;
#18967 = CARTESIAN_POINT ( 'NONE',  ( -22.27502019258949417, 422.2448905683720568, -15.47720386886985544 ) ) ;
#18968 = CARTESIAN_POINT ( 'NONE',  ( 60.03793209889851568, 30.52886280891152282, -126.1729372809868863 ) ) ;
#18969 = VECTOR ( 'NONE', #12497, 1000.000000000000000 ) ;
#18970 = DIRECTION ( 'NONE',  ( 0.000000000000000000, 0.000000000000000000, 1.000000000000000000 ) ) ;
#18971 = CARTESIAN_POINT ( 'NONE',  ( -22.27502019258949062, 466.9948905683720000, 15.47720386886985189 ) ) ;
#18972 = VERTEX_POINT ( 'NONE', #19119 ) ;
#18973 = CARTESIAN_POINT ( 'NONE',  ( -14.48388495494901029, 469.8073905683719431, -9.489475012073734561 ) ) ;
#18974 = CARTESIAN_POINT ( 'NONE',  ( 0.5805565836007611225, 3.752776749732563477, 6.500000000000000000 ) ) ;
#18975 = CARTESIAN_POINT ( 'NONE',  ( -11.73070664223725501, 397.9323905765656377, -11.32908994701042715 ) ) ;
#18976 = CARTESIAN_POINT ( 'NONE',  ( -40.01497788969913216, 280.4323905765655809, -16.95518130045146421 ) ) ;
#18977 = CARTESIAN_POINT ( 'NONE',  ( -40.01497788969912506, 298.8073905601785327, 16.95518130045146776 ) ) ;
#18978 = CARTESIAN_POINT ( 'NONE',  ( 0.2573354458087861452, -4.368923434677201456, -5.432802636760778903 ) ) ;
#18979 = DIRECTION ( 'NONE',  ( -0.9283449136418786551, 0.000000000000000000, 0.3717199501173604204 ) ) ;
#18980 = AXIS2_PLACEMENT_3D ( 'NONE', #13646, #5197, #12008 ) ;
#18981 = DIRECTION ( 'NONE',  ( 0.000000000000000000, 0.000000000000000000, 1.000000000000000000 ) ) ;
#18982 = CARTESIAN_POINT ( 'NONE',  ( -45.64106924314016567, 238.1823905601784759, 11.32908994701042538 ) ) ;
#18983 = DIRECTION ( 'NONE',  ( -1.000000000000000000, 0.000000000000000000, 0.000000000000000000 ) ) ;
#18984 =( BOUNDED_CURVE ( )  B_SPLINE_CURVE ( 2, ( #19434, #19328, #7747, #17705, #2902, #16416, #12844, #9482, #17810, #15996, #13167, #12951, #6339, #8062, #4514, #1272, #7851 ),
 .UNSPECIFIED., .F., .T. ) 
 B_SPLINE_CURVE_WITH_KNOTS ( ( 3, 2, 2, 2, 2, 2, 2, 2, 3 ),
 ( 0.9062500000000001110, 0.9082031250000001110, 0.9101562500000001110, 0.9121093750000001110, 0.9140625000000001110, 0.9160156250000001110, 0.9179687500000001110, 0.9199218750000001110, 0.9218750000000001110 ),
 .UNSPECIFIED. ) 
 CURVE ( )  GEOMETRIC_REPRESENTATION_ITEM ( )  RATIONAL_B_SPLINE_CURVE ( ( 0.9999999999999988898, 0.9807852804032315408, 1.000000000000000000, 0.9807852804032304306, 1.000000000000000000, 0.9807852804032304306, 1.000000000000000000, 0.9807852804032304306, 1.000000000000000000, 0.9807852804032304306, 1.000000000000000000, 0.9807852804032304306, 1.000000000000000000, 0.9807852804032304306, 1.000000000000000000, 0.9807852804032293204, 1.000000000000001110 ) ) 
 REPRESENTATION_ITEM ( '' )  );
#18985 = CARTESIAN_POINT ( 'NONE',  ( -16.84014894278197616, 279.1198905683720568, 11.84573899990672530 ) ) ;
#18986 = CARTESIAN_POINT ( 'NONE',  ( -47.16347859291443001, 246.6198905601784759, -7.653668647301793193 ) ) ;
#18987 = CARTESIAN_POINT ( 'NONE',  ( -32.66413529028187668, 404.1823905765656946, 19.99999999999999289 ) ) ;
#18988 = CARTESIAN_POINT ( 'NONE',  ( -40.53162694259544452, 424.1198905683720000, -11.84573899990672707 ) ) ;
#18989 = CARTESIAN_POINT ( 'NONE',  ( -48.68588794268873698, 573.2448905601785327, 0.000000000000000000 ) ) ;
#18990 = CARTESIAN_POINT ( 'NONE',  ( -32.01814843081343298, 263.1823905683720000, -16.75240474999999307 ) ) ;
#18991 = ORIENTED_EDGE ( 'NONE', *, *, #16959, .T. ) ;
#18992 = CARTESIAN_POINT ( 'NONE',  ( -45.64106924314019409, 481.0573905765655240, -11.32908994701042538 ) ) ;
#18993 = ORIENTED_EDGE ( 'NONE', *, *, #7376, .T. ) ;
#18994 = CARTESIAN_POINT ( 'NONE',  ( -45.43829269268872650, 475.6823905683719431, 3.332260488124734632 ) ) ;
#18995 = EDGE_CURVE ( 'NONE', #1524, #10342, #17393, .T. ) ;
#18996 = ORIENTED_EDGE ( 'NONE', *, *, #2802, .T. ) ;
#18997 = CARTESIAN_POINT ( 'NONE',  ( -203.6858879426887654, 575.7448905601785327, 2.143131898507868248E-14 ) ) ;
#18998 = CARTESIAN_POINT ( 'NONE',  ( -44.16309181155855157, 234.4948905683720284, 6.410867750099241924 ) ) ;
#18999 = ORIENTED_EDGE ( 'NONE', *, *, #20596, .T. ) ;
#19000 = CARTESIAN_POINT ( 'NONE',  ( -28.68588794268873698, 531.3698905683720568, -16.75240474999999307 ) ) ;
#19001 = CARTESIAN_POINT ( 'NONE',  ( -71.26501780185373036, 205.1437886375728965, 0.000000000000000000 ) ) ;
#19002 = CARTESIAN_POINT ( 'NONE',  ( -32.66413529028189089, 469.8073905765656377, -19.99999999999999289 ) ) ;
#19003 = PLANE ( 'NONE',  #21362 ) ;
#19004 = CARTESIAN_POINT ( 'NONE',  ( -10.20829729246297646, 286.3698905765655809, 7.653668647301790529 ) ) ;
#19005 = AXIS2_PLACEMENT_3D ( 'NONE', #10634, #20496, #15638 ) ;
#19006 = CARTESIAN_POINT ( 'NONE',  ( -24.70764059509556887, 454.4323905601784759, -19.99999999999999289 ) ) ;
#19007 = LINE ( 'NONE', #14158, #3593 ) ;
#19008 = AXIS2_PLACEMENT_3D ( 'NONE', #14873, #18097, #9866 ) ;
#19009 = EDGE_CURVE ( 'NONE', #18802, #3367, #15278, .T. ) ;
#19010 = CARTESIAN_POINT ( 'NONE',  ( -22.27502019258950128, 512.2448905683720568, -15.47720386886985544 ) ) ;
#19011 = CARTESIAN_POINT ( 'NONE',  ( -162.2727221670389781, 30.52886280891152282, -4.999999999999990230 ) ) ;
#19012 = CARTESIAN_POINT ( 'NONE',  ( -11.93348319268870661, 238.8698905683720568, -2.051577885510841163E-15 ) ) ;
#19013 = CARTESIAN_POINT ( 'NONE',  ( -16.84014894278198682, 341.6198905683720000, -11.84573899990672707 ) ) ;
#19014 = CARTESIAN_POINT ( 'NONE',  ( -8.685887942688735208, 472.2448905601784759, -2.449293598294705724E-15 ) ) ;
#19015 = VECTOR ( 'NONE', #8249, 1000.000000000000000 ) ;
#19016 = CARTESIAN_POINT ( 'NONE',  ( -36.33955658999051508, 359.1198905601785327, 18.47759065022572500 ) ) ;
#19017 = CIRCLE ( 'NONE', #9349, 10.00000000000000533 ) ;
#19018 = CARTESIAN_POINT ( 'NONE',  ( -45.43829269268870519, 384.1823905683720000, 3.332260488124734632 ) ) ;
#19019 = CIRCLE ( 'NONE', #10373, 125.0000000000000000 ) ;
#19020 = DIRECTION ( 'NONE',  ( 0.000000000000000000, 0.000000000000000000, 1.000000000000000000 ) ) ;
#19021 = VECTOR ( 'NONE', #16540, 1000.000000000000000 ) ;
#19022 = CARTESIAN_POINT ( 'NONE',  ( -42.82802356641965957, 378.4948905601784759, 14.14213562373094923 ) ) ;
#19023 = ORIENTED_EDGE ( 'NONE', *, *, #19589, .F. ) ;
#19024 = CARTESIAN_POINT ( 'NONE',  ( -24.70764059509555821, 349.1823905765655809, -19.99999999999999289 ) ) ;
#19025 = ORIENTED_EDGE ( 'NONE', *, *, #7856, .T. ) ;
#19026 = CARTESIAN_POINT ( 'NONE',  ( -28.68588794268873343, 502.8698905683719431, -16.75240474999999307 ) ) ;
#19027 = CARTESIAN_POINT ( 'NONE',  ( -22.62331590640576451, 135.1716627696692683, 11.80838889663595914 ) ) ;
#19028 = VECTOR ( 'NONE', #12731, 1000.000000000000000 ) ;
#19029 = ORIENTED_EDGE ( 'NONE', *, *, #7307, .F. ) ;
#19030 = CARTESIAN_POINT ( 'NONE',  ( -40.53162694259543031, 296.6198905683720000, 11.84573899990672885 ) ) ;
#19031 =( GEOMETRIC_REPRESENTATION_CONTEXT ( 3 ) GLOBAL_UNCERTAINTY_ASSIGNED_CONTEXT ( ( #20454 ) ) GLOBAL_UNIT_ASSIGNED_CONTEXT ( ( #5224, #5009, #18200 ) ) REPRESENTATION_CONTEXT ( 'NONE', 'WORKASPACE' ) );
#19032 = VERTEX_POINT ( 'NONE', #4513 ) ;
#19033 = CARTESIAN_POINT ( 'NONE',  ( -13.20868407381885667, 348.2448905683720000, 6.410867750099229490 ) ) ;
#19034 = CARTESIAN_POINT ( 'NONE',  ( -25.35362745456398770, 341.0573905683720568, -16.75240474999999307 ) ) ;
#19035 = VECTOR ( 'NONE', #13703, 1000.000000000000000 ) ;
#19036 = CARTESIAN_POINT ( 'NONE',  ( -11.73070664223724080, 277.9323905765655809, -11.32908994701042715 ) ) ;
#19037 = COLOUR_RGB ( '',0.7921568627450980005, 0.8196078431372548767, 0.9333333333333333481 ) ;
#19038 = DIRECTION ( 'NONE',  ( -1.000000000000000000, 0.000000000000000000, 0.000000000000000000 ) ) ;
#19039 = CARTESIAN_POINT ( 'NONE',  ( -16.84014894278197616, 240.1198905683720284, -11.84573899990672707 ) ) ;
#19040 = LINE ( 'NONE', #4224, #16036 ) ;
#19041 = CARTESIAN_POINT ( 'NONE',  ( -28.68588794268871567, 387.8698905683720000, 16.75240474999999307 ) ) ;
#19042 = DIRECTION ( 'NONE',  ( -1.000000000000000000, -0.000000000000000000, -0.000000000000000000 ) ) ;
#19043 = DIRECTION ( 'NONE',  ( 1.000000000000000000, 0.000000000000000000, 0.000000000000000000 ) ) ;
#19044 = CIRCLE ( 'NONE', #12487, 4.000000000000001776 ) ;
#19045 = DIRECTION ( 'NONE',  ( 0.000000000000000000, 0.000000000000000000, 1.000000000000000000 ) ) ;
#19046 = CARTESIAN_POINT ( 'NONE',  ( -40.53162694259544452, 445.1198905683720568, 11.84573899990672885 ) ) ;
#19047 = ORIENTED_EDGE ( 'NONE', *, *, #6927, .F. ) ;
#19048 = CARTESIAN_POINT ( 'NONE',  ( -40.01497788969915348, 455.6823905601785327, -16.95518130045146421 ) ) ;
#19049 = VERTEX_POINT ( 'NONE', #12843 ) ;
#19050 = VERTEX_POINT ( 'NONE', #1379 ) ;
#19051 = ORIENTED_EDGE ( 'NONE', *, *, #13718, .T. ) ;
#19052 = FACE_OUTER_BOUND ( 'NONE', #4576, .T. ) ;
#19053 = CIRCLE ( 'NONE', #10750, 10.00000000000000888 ) ;
#19054 = CARTESIAN_POINT ( 'NONE',  ( -21.03221929538691981, 334.1198905601784759, -18.47759065022572855 ) ) ;
#19055 = EDGE_CURVE ( 'NONE', #10285, #2137, #6127, .T. ) ;
#19056 = CARTESIAN_POINT ( 'NONE',  ( -16.84014894278197971, 297.6198905683720000, 11.84573899990672530 ) ) ;
#19057 = CARTESIAN_POINT ( 'NONE',  ( -19.19641293061497933, 358.8073905683720000, 14.20200298773971426 ) ) ;
#19058 = CARTESIAN_POINT ( 'NONE',  ( -24.70764059509555111, 294.4323905601784190, -19.99999999999999289 ) ) ;
#19059 = EDGE_CURVE ( 'NONE', #16623, #7807, #6659, .T. ) ;
#19060 = CARTESIAN_POINT ( 'NONE',  ( -48.68588794268872988, 522.3073905765655809, 3.978247347593168115 ) ) ;
#19061 = CARTESIAN_POINT ( 'NONE',  ( -22.27502019258949417, 410.7448905683720568, -15.47720386886985544 ) ) ;
#19062 = CARTESIAN_POINT ( 'NONE',  ( -19.19641293061496867, 248.8073905683720284, 14.20200298773971426 ) ) ;
#19063 = CARTESIAN_POINT ( 'NONE',  ( -14.48388495494900674, 407.9323905683719431, 9.489475012073731008 ) ) ;
#19064 = CARTESIAN_POINT ( 'NONE',  ( -21.03221929538692336, 348.8698905765656377, -18.47759065022572855 ) ) ;
#19065 = CARTESIAN_POINT ( 'NONE',  ( -8.685887942688710339, 262.2448905601784759, -2.449293598294705724E-15 ) ) ;
#19066 = CARTESIAN_POINT ( 'NONE',  ( -40.53162694259543031, 312.6198905683720000, -11.84573899990672707 ) ) ;
#19067 =( NAMED_UNIT ( * ) PLANE_ANGLE_UNIT ( ) SI_UNIT ( $, .RADIAN. ) );
#19068 = CARTESIAN_POINT ( 'NONE',  ( -45.43829269268871940, 465.6823905683720000, 3.332260488124734632 ) ) ;
#19069 = CARTESIAN_POINT ( 'NONE',  ( -47.16347859291446554, 512.6198905765656946, 7.653668647301805628 ) ) ;
#19070 = CARTESIAN_POINT ( 'NONE',  ( -8.685887942688902186, 371.9323905601784759, 3.978247347593586447 ) ) ;
#19071 = CARTESIAN_POINT ( 'NONE',  ( -8.685887942688742314, 573.2448905601785327, 2.449293598294706119E-15 ) ) ;
#19072 = CARTESIAN_POINT ( 'NONE',  ( -28.68588794268871567, 372.8698905683720000, -16.75240474999999307 ) ) ;
#19073 = CARTESIAN_POINT ( 'NONE',  ( -25.35362745456399836, 496.6823905683721136, 16.75240474999998952 ) ) ;
#19074 = CARTESIAN_POINT ( 'NONE',  ( -21.03221929538694113, 514.1198905601785327, -18.47759065022572855 ) ) ;
#19075 = CARTESIAN_POINT ( 'NONE',  ( -28.68588794268871567, 351.3698905683720568, -16.75240474999999307 ) ) ;
#19076 = ADVANCED_FACE ( 'NONE', ( #4302 ), #7530, .T. ) ;
#19077 = VERTEX_POINT ( 'NONE', #2682 ) ;
#19078 = CARTESIAN_POINT ( 'NONE',  ( -35.09675569278797269, 505.7448905683720000, 15.47720386886985366 ) ) ;
#19079 = ORIENTED_EDGE ( 'NONE', *, *, #17553, .F. ) ;
#19080 = CARTESIAN_POINT ( 'NONE',  ( -21.03221929538690560, 315.1198905765656377, 18.47759065022572500 ) ) ;
#19081 = CARTESIAN_POINT ( 'NONE',  ( -28.68588794268872277, 422.8698905683720568, -16.75240474999999307 ) ) ;
#19082 = CARTESIAN_POINT ( 'NONE',  ( 20.42502041961813930, 230.5765313837437418, -60.00000000000000000 ) ) ;
#19083 = FACE_OUTER_BOUND ( 'NONE', #18191, .T. ) ;
#19084 = CARTESIAN_POINT ( 'NONE',  ( -40.53162694259545162, 462.6198905683720000, -11.84573899990672707 ) ) ;
#19085 = CIRCLE ( 'NONE', #450, 4.000000000000001776 ) ;
#19086 = ORIENTED_EDGE ( 'NONE', *, *, #4146, .T. ) ;
#19087 = CARTESIAN_POINT ( 'NONE',  ( -38.17536295476246977, 472.3073905683720568, -14.20200298773971426 ) ) ;
#19088 = CARTESIAN_POINT ( 'NONE',  ( -24.70764059509553334, 250.0573905601785043, 19.99999999999998934 ) ) ;
#19089 = CARTESIAN_POINT ( 'NONE',  ( -36.33955658999052218, 393.8698905765656377, 18.47759065022572500 ) ) ;
#19090 = CARTESIAN_POINT ( 'NONE',  ( -8.685887942688712116, 282.2448905601784759, -2.449293598294705724E-15 ) ) ;
#19091 = CARTESIAN_POINT ( 'NONE',  ( 65.85920792673738333, 160.1716627696692683, 40.00000000000000000 ) ) ;
#19092 = LINE ( 'NONE', #939, #12208 ) ;
#19093 = DIRECTION ( 'NONE',  ( 0.000000000000000000, -0.000000000000000000, 1.000000000000000000 ) ) ;
#19094 = EDGE_CURVE ( 'NONE', #10871, #21097, #20150, .T. ) ;
#19095 = PLANE ( 'NONE',  #13722 ) ;
#19096 = CARTESIAN_POINT ( 'NONE',  ( -10.20829729246297291, 241.6198905601784759, 7.653668647301790529 ) ) ;
#19097 = DIRECTION ( 'NONE',  ( 0.000000000000000000, 0.000000000000000000, 1.000000000000000000 ) ) ;
#19098 = CIRCLE ( 'NONE', #12180, 10.00000000000000888 ) ;
#19099 = CARTESIAN_POINT ( 'NONE',  ( -32.01814843081343298, 273.1823905683720568, -16.75240474999999307 ) ) ;
#19100 = CARTESIAN_POINT ( 'NONE',  ( -32.66413529028186247, 249.4323905601784475, 19.99999999999999289 ) ) ;
#19101 = CARTESIAN_POINT ( 'NONE',  ( -162.2727221670389781, 30.52886280891152282, 0.000000000000000000 ) ) ;
#19102 = CARTESIAN_POINT ( 'NONE',  ( -16.84014894278199748, 421.6198905683720000, -11.84573899990672707 ) ) ;
#19103 = CYLINDRICAL_SURFACE ( 'NONE', #10584, 28.29169339157297358 ) ;
#19104 = CARTESIAN_POINT ( 'NONE',  ( -16.84014894278197616, 251.6198905683720284, -11.84573899990672707 ) ) ;
#19105 = ADVANCED_FACE ( 'NONE', ( #15884 ), #9266, .T. ) ;
#19106 = B_SPLINE_CURVE_WITH_KNOTS ( 'NONE', 3,
 ( #20062, #16611, #1801, #11835, #2320, #7163, #8900, #12155, #20374, #15311, #5658, #2111, #5758, #3931, #13786, #18633, #17139, #814, #5549, #7382, #18845, #3823 ),
 .UNSPECIFIED., .F., .F.,
 ( 4, 2, 2, 2, 2, 2, 2, 2, 2, 2, 4 ),
 ( 0.000000000000000000, 0.002281693049900210702, 0.003422539574850314101, 0.004563386099800417935, 0.006845079149700616060, 0.009126772199600815053, 0.01140846524950101318, 0.01254931177445110617, 0.01369015829940119916, 0.01597185134930136780, 0.01825354439920153643 ),
 .UNSPECIFIED. ) ;
#19107 = ORIENTED_EDGE ( 'NONE', *, *, #958, .T. ) ;
#19108 = CARTESIAN_POINT ( 'NONE',  ( -36.33955658999052218, 480.1198905765656377, -18.47759065022572855 ) ) ;
#19109 = ORIENTED_EDGE ( 'NONE', *, *, #10920, .T. ) ;
#19110 = CARTESIAN_POINT ( 'NONE',  ( -40.53162694259545162, 484.1198905683720000, -11.84573899990672707 ) ) ;
#19111 = ORIENTED_EDGE ( 'NONE', *, *, #1121, .F. ) ;
#19112 = CYLINDRICAL_SURFACE ( 'NONE', #20397, 19.99999999999999645 ) ;
#19113 = CARTESIAN_POINT ( 'NONE',  ( -25.35362745456396638, 246.6823905683720284, 16.75240474999998952 ) ) ;
#19114 = ORIENTED_EDGE ( 'NONE', *, *, #20396, .F. ) ;
#19115 = CARTESIAN_POINT ( 'NONE',  ( -11.93348319268874036, 519.1823905683720568, -3.332260488124732856 ) ) ;
#19116 = CARTESIAN_POINT ( 'NONE',  ( -5.502341142637721561, 600.7448905601785327, -7.573322868991255952 ) ) ;
#19117 = CARTESIAN_POINT ( 'NONE',  ( -21.03221929538693402, 458.8698905765656377, -18.47759065022572855 ) ) ;
#19118 = CARTESIAN_POINT ( 'NONE',  ( 32.47532367400570763, 585.7448905601785327, 163.9643442751439295 ) ) ;
#19119 = CARTESIAN_POINT ( 'NONE',  ( -8.685887942688713892, 292.2448905601784759, -2.449293598294705724E-15 ) ) ;
#19120 = CARTESIAN_POINT ( 'NONE',  ( -27.59433460082644274, 223.9102039777117170, -18.70402771398575226 ) ) ;
#19121 = CARTESIAN_POINT ( 'NONE',  ( -22.27502019258945865, 228.4948905683720284, 15.47720386886985189 ) ) ;
#19122 =( BOUNDED_CURVE ( )  B_SPLINE_CURVE ( 2, ( #16009, #1191, #12961, #7761, #14388, #20972, #6140, #12751, #11115, #19551, #17923, #9169, #5557, #3230, #12052, #10023, #1500 ),
 .UNSPECIFIED., .F., .T. ) 
 B_SPLINE_CURVE_WITH_KNOTS ( ( 3, 2, 2, 2, 2, 2, 2, 2, 3 ),
 ( 0.9375000000000001110, 0.9394531250000001110, 0.9414062500000001110, 0.9433593750000001110, 0.9453125000000001110, 0.9472656250000001110, 0.9492187500000001110, 0.9511718750000001110, 0.9531250000000001110 ),
 .UNSPECIFIED. ) 
 CURVE ( )  GEOMETRIC_REPRESENTATION_ITEM ( )  RATIONAL_B_SPLINE_CURVE ( ( 0.9999999999999988898, 0.9807852804032315408, 1.000000000000000000, 0.9807852804032304306, 1.000000000000000000, 0.9807852804032304306, 1.000000000000000000, 0.9807852804032304306, 1.000000000000000000, 0.9807852804032304306, 1.000000000000000000, 0.9807852804032304306, 1.000000000000000000, 0.9807852804032304306, 1.000000000000000000, 0.9807852804032293204, 1.000000000000001110 ) ) 
 REPRESENTATION_ITEM ( '' )  );
#19123 = CARTESIAN_POINT ( 'NONE',  ( -22.27502019258949417, 518.4948905683719431, 15.47720386886985189 ) ) ;
#19124 = CARTESIAN_POINT ( 'NONE',  ( -48.68588794268873698, 573.2448905601785327, 0.000000000000000000 ) ) ;
#19125 = CARTESIAN_POINT ( 'NONE',  ( -45.43829269268869808, 223.8698905683720284, 0.000000000000000000 ) ) ;
#19126 = CARTESIAN_POINT ( 'NONE',  ( -32.01814843081344719, 333.1823905683720000, -16.75240474999999307 ) ) ;
#19127 = AXIS2_PLACEMENT_3D ( 'NONE', #11549, #18139, #6672 ) ;
#19128 = CARTESIAN_POINT ( 'NONE',  ( -24.70764059509556176, 470.0573905601784759, 19.99999999999998934 ) ) ;
#19129 = CARTESIAN_POINT ( 'NONE',  ( -48.68588794268870146, 271.9948905765656377, 0.000000000000000000 ) ) ;
#19130 = AXIS2_PLACEMENT_3D ( 'NONE', #669, #5516, #7235 ) ;
#19131 = CARTESIAN_POINT ( 'NONE',  ( -11.93348319268872260, 379.1823905683721136, -3.332260488124732856 ) ) ;
#19132 = CARTESIAN_POINT ( 'NONE',  ( -48.68588794268870146, 321.9948905765655809, 0.000000000000000000 ) ) ;
#19133 = EDGE_CURVE ( 'NONE', #364, #1064, #9586, .T. ) ;
#19134 = CARTESIAN_POINT ( 'NONE',  ( -48.68588794268870856, 377.5573905601785327, 3.978247347593168115 ) ) ;
#19135 = EDGE_CURVE ( 'NONE', #8982, #1192, #8390, .T. ) ;
#19136 = ORIENTED_EDGE ( 'NONE', *, *, #16330, .T. ) ;
#19137 = DIRECTION ( 'NONE',  ( 0.000000000000000000, 0.000000000000000000, -1.000000000000000000 ) ) ;
#19138 = VERTEX_POINT ( 'NONE', #5805 ) ;
#19139 = ORIENTED_EDGE ( 'NONE', *, *, #4537, .T. ) ;
#19140 = CARTESIAN_POINT ( 'NONE',  ( -32.01814843081346140, 503.1823905683721136, -16.75240474999999307 ) ) ;
#19141 = MANIFOLD_SOLID_BREP ( 'Cut-Extrude6[1]', #12097 ) ;
#19142 = CARTESIAN_POINT ( 'NONE',  ( -8.685887942688715668, 296.9948905765655809, -2.449293598294705724E-15 ) ) ;
#19143 = ORIENTED_EDGE ( 'NONE', *, *, #8010, .F. ) ;
#19144 = CARTESIAN_POINT ( 'NONE',  ( -35.09675569278794427, 297.2448905683720000, 15.47720386886985366 ) ) ;
#19145 = EDGE_LOOP ( 'NONE', ( #3525, #6421, #4395 ) ) ;
#19146 = CARTESIAN_POINT ( 'NONE',  ( -19.19641293061497933, 327.3073905683720568, 14.20200298773971426 ) ) ;
#19147 = CARTESIAN_POINT ( 'NONE',  ( -14.48388495494899608, 347.9323905683720568, 9.489475012073731008 ) ) ;
#19148 = AXIS2_PLACEMENT_3D ( 'NONE', #1074, #10992, #9379 ) ;
#19149 = EDGE_CURVE ( 'NONE', #16828, #6455, #9377, .T. ) ;
#19150 = CARTESIAN_POINT ( 'NONE',  ( -14.54375231895775755, 258.2448905765656377, -14.14213562373094746 ) ) ;
#19151 = CARTESIAN_POINT ( 'NONE',  ( -48.68588794268872277, 501.9948905765656377, 0.000000000000000000 ) ) ;
#19152 = CARTESIAN_POINT ( 'NONE',  ( -11.93348319268870661, 249.1823905683720568, -3.332260488124732856 ) ) ;
#19153 = CARTESIAN_POINT ( 'NONE',  ( -32.66413529028185536, 225.0573905601784759, -19.99999999999999289 ) ) ;
#19154 = CARTESIAN_POINT ( 'NONE',  ( -38.17536295476245556, 406.9323905683719431, 14.20200298773971781 ) ) ;
#19155 = ADVANCED_FACE ( 'NONE', ( #13384 ), #21378, .T. ) ;
#19156 = CARTESIAN_POINT ( 'NONE',  ( 88.28695088269886071, 152.5259582928263740, -20.00000000000000355 ) ) ;
#19157 = FACE_OUTER_BOUND ( 'NONE', #19342, .T. ) ;
#19158 = CARTESIAN_POINT ( 'NONE',  ( -14.54375231895775578, 243.4948905601784759, -14.14213562373094746 ) ) ;
#19159 = CARTESIAN_POINT ( 'NONE',  ( -13.20868407381887089, 449.4948905683720568, -6.410867750099233042 ) ) ;
#19160 = EDGE_LOOP ( 'NONE', ( #12752, #18932 ) ) ;
#19161 = CARTESIAN_POINT ( 'NONE',  ( -42.82802356641966668, 445.9948905601784759, -14.14213562373094746 ) ) ;
#19162 = EDGE_CURVE ( 'NONE', #13267, #19049, #14585, .T. ) ;
#19163 = VERTEX_POINT ( 'NONE', #3320 ) ;
#19164 = EDGE_LOOP ( 'NONE', ( #15472, #16835, #1373 ) ) ;
#19165 = DIRECTION ( 'NONE',  ( -0.9864615503757148129, 0.000000000000000000, 0.1639927121256942455 ) ) ;
#19166 = CARTESIAN_POINT ( 'NONE',  ( -8.685887942688717445, 322.2448905601784759, -2.449293598294705724E-15 ) ) ;
#19167 = CARTESIAN_POINT ( 'NONE',  ( -25.35362745456398059, 358.1823905683720000, 16.75240474999998952 ) ) ;
#19168 = CARTESIAN_POINT ( 'NONE',  ( 0.05533025579362401553, -6.264553569211847694, 2.149474931388141385 ) ) ;
#19169 = CARTESIAN_POINT ( 'NONE',  ( -48.68588794268872277, 501.6823905765655809, -3.978247347593158345 ) ) ;
#19170 = CARTESIAN_POINT ( 'NONE',  ( -13.20868407381886200, 379.4948905683720000, -6.410867750099233042 ) ) ;
#19171 = CARTESIAN_POINT ( 'NONE',  ( -38.17536295476243424, 236.9323905683720000, 14.20200298773971781 ) ) ;
#19172 = CARTESIAN_POINT ( 'NONE',  ( -32.01814843081344719, 401.6823905683720000, -16.75240474999999307 ) ) ;
#19173 = CARTESIAN_POINT ( 'NONE',  ( -8.685887942688719221, 336.6823905765656377, 3.978247347593161010 ) ) ;
#19174 = CARTESIAN_POINT ( 'NONE',  ( -8.685887942688539809, 322.5573905601784190, -3.978247347592740013 ) ) ;
#19175 = CARTESIAN_POINT ( 'NONE',  ( -38.17536295476244845, 312.3073905683720568, -14.20200298773971426 ) ) ;
#19176 = CARTESIAN_POINT ( 'NONE',  ( -19.19641293061499354, 451.9323905683720568, -14.20200298773971603 ) ) ;
#19177 = CARTESIAN_POINT ( 'NONE',  ( -45.64106924314019409, 458.1823905601784190, 11.32908994701042538 ) ) ;
#19178 = DIRECTION ( 'NONE',  ( 0.000000000000000000, 0.000000000000000000, -1.000000000000000000 ) ) ;
#19179 = DIRECTION ( 'NONE',  ( -1.000000000000000000, -0.000000000000000000, 0.000000000000000000 ) ) ;
#19180 = CARTESIAN_POINT ( 'NONE',  ( -11.93348319268872260, 360.6823905683720568, -3.332260488124732856 ) ) ;
#19181 = CARTESIAN_POINT ( 'NONE',  ( -32.01814843081346851, 506.0573905683719431, 16.75240474999999307 ) ) ;
#19182 = EDGE_CURVE ( 'NONE', #2882, #15103, #8061, .T. ) ;
#19183 = CARTESIAN_POINT ( 'NONE',  ( -36.33955658999052218, 505.3698905601784190, -18.47759065022572855 ) ) ;
#19184 = CARTESIAN_POINT ( 'NONE',  ( -40.53162694259543031, 325.1198905683720568, 11.84573899990672885 ) ) ;
#19185 = ORIENTED_EDGE ( 'NONE', *, *, #18607, .F. ) ;
#19186 = CARTESIAN_POINT ( 'NONE',  ( -40.53162694259545162, 495.1198905683720000, 11.84573899990672885 ) ) ;
#19187 = ORIENTED_EDGE ( 'NONE', *, *, #15407, .F. ) ;
#19188 = FACE_OUTER_BOUND ( 'NONE', #20786, .T. ) ;
#19189 = CARTESIAN_POINT ( 'NONE',  ( -44.16309181155857289, 425.9948905683720568, 6.410867750099241924 ) ) ;
#19190 = DIRECTION ( 'NONE',  ( 1.000000000000000000, 1.250996701150283068E-16, -0.000000000000000000 ) ) ;
#19191 = SURFACE_SIDE_STYLE ('',( #12599 ) ) ;
#19192 = CARTESIAN_POINT ( 'NONE',  ( -19.19641293061499354, 460.4323905683721136, -14.20200298773971603 ) ) ;
#19193 = VERTEX_POINT ( 'NONE', #3214 ) ;
#19194 = CARTESIAN_POINT ( 'NONE',  ( -40.53162694259545162, 475.1198905683720000, 11.84573899990672885 ) ) ;
#19195 = CARTESIAN_POINT ( 'NONE',  ( -10.20829729246297291, 246.3698905765656093, 7.653668647301790529 ) ) ;
#19196 = CARTESIAN_POINT ( 'NONE',  ( -48.68588794268871567, 411.9948905765656377, 0.000000000000000000 ) ) ;
#19197 = CARTESIAN_POINT ( 'NONE',  ( -21.03221929538691271, 278.8698905765656377, -18.47759065022572855 ) ) ;
#19198 = DIRECTION ( 'NONE',  ( 0.000000000000000000, 0.000000000000000000, 1.000000000000000000 ) ) ;
#19199 = CARTESIAN_POINT ( 'NONE',  ( -10.20829729246299600, 437.6198905765656377, -7.653668647301794969 ) ) ;
#19200 = DIRECTION ( 'NONE',  ( 0.000000000000000000, 0.000000000000000000, 1.000000000000000000 ) ) ;
#19201 = ADVANCED_FACE ( 'NONE', ( #1593 ), #19752, .T. ) ;
#19202 = LINE ( 'NONE', #1051, #9209 ) ;
#19203 = CARTESIAN_POINT ( 'NONE',  ( -45.56270947133124594, 223.9102039777115749, 4.062575975128698502 ) ) ;
#19204 = CARTESIAN_POINT ( 'NONE',  ( -8.685887942688708563, 242.2448905601785043, -2.449293598294705724E-15 ) ) ;
#19205 = FACE_OUTER_BOUND ( 'NONE', #2457, .T. ) ;
#19206 = CARTESIAN_POINT ( 'NONE',  ( -45.43829269268871229, 425.6823905683720568, 3.332260488124734632 ) ) ;
#19207 = CARTESIAN_POINT ( 'NONE',  ( -10.20829729246298712, 382.8698905601784759, -7.653668647301794969 ) ) ;
#19208 = CARTESIAN_POINT ( 'NONE',  ( -11.93348319268870839, 250.6823905683720852, -3.332260488124732856 ) ) ;
#19209 = EDGE_LOOP ( 'NONE', ( #19417, #17745 ) ) ;
#19210 = ORIENTED_EDGE ( 'NONE', *, *, #19579, .T. ) ;
#19211 = FACE_OUTER_BOUND ( 'NONE', #17873, .T. ) ;
#19212 = ORIENTED_EDGE ( 'NONE', *, *, #16923, .T. ) ;
#19213 = CARTESIAN_POINT ( 'NONE',  ( -14.48388495494901029, 471.3073905683720568, -9.489475012073734561 ) ) ;
#19214 = ADVANCED_FACE ( 'NONE', ( #5151 ), #8164, .T. ) ;
#19215 = ORIENTED_EDGE ( 'NONE', *, *, #21057, .F. ) ;
#19216 = DIRECTION ( 'NONE',  ( 1.374938938973709817E-16, -1.000000000000000000, 0.000000000000000000 ) ) ;
#19217 = CARTESIAN_POINT ( 'NONE',  ( -32.01814843081343298, 236.0573905683720284, 16.75240474999999307 ) ) ;
#19218 = ORIENTED_EDGE ( 'NONE', *, *, #6116, .F. ) ;
#19219 = CARTESIAN_POINT ( 'NONE',  ( -44.16309181155859420, 533.2448905683719431, -6.410867750099231266 ) ) ;
#19220 = CARTESIAN_POINT ( 'NONE',  ( 0.000000000000000000, 0.000000000000000000, 0.000000000000000000 ) ) ;
#19221 = AXIS2_PLACEMENT_3D ( 'NONE', #3479, #14855, #14747 ) ;
#19222 = CARTESIAN_POINT ( 'NONE',  ( -10.20829729246299955, 467.6198905765656377, -7.653668647301794969 ) ) ;
#19223 = DIRECTION ( 'NONE',  ( -0.000000000000000000, -0.000000000000000000, 1.000000000000000000 ) ) ;
#19224 = CARTESIAN_POINT ( 'NONE',  ( -42.82802356641965247, 283.2448905765656377, 14.14213562373094923 ) ) ;
#19225 = CARTESIAN_POINT ( 'NONE',  ( -28.49465132804630940, 223.9102039777116602, -18.60448546972727257 ) ) ;
#19226 = CARTESIAN_POINT ( 'NONE',  ( 5.074999999999999289, -7.505553499465148271, 0.000000000000000000 ) ) ;
#19227 = EDGE_CURVE ( 'NONE', #18805, #4636, #8273, .T. ) ;
#19228 = VECTOR ( 'NONE', #865, 1000.000000000000000 ) ;
#19229 = CARTESIAN_POINT ( 'NONE',  ( -19.19641293061496867, 237.3073905683720284, 14.20200298773971426 ) ) ;
#19230 = CARTESIAN_POINT ( 'NONE',  ( -13.20868407381885490, 329.7448905683720568, 6.410867750099229490 ) ) ;
#19231 = CARTESIAN_POINT ( 'NONE',  ( 0.000000000000000000, 0.000000000000000000, 0.000000000000000000 ) ) ;
#19232 = DIRECTION ( 'NONE',  ( -1.191790137725560488E-16, 1.000000000000000000, -0.000000000000000000 ) ) ;
#19233 = CARTESIAN_POINT ( 'NONE',  ( -38.17536295476244845, 303.8073905683720000, -14.20200298773971426 ) ) ;
#19234 = CARTESIAN_POINT ( 'NONE',  ( -19.19641293061498999, 390.4323905683720568, -14.20200298773971603 ) ) ;
#19235 = CARTESIAN_POINT ( 'NONE',  ( -19.19641293061500065, 528.8073905683720568, 14.20200298773971426 ) ) ;
#19236 = CARTESIAN_POINT ( 'NONE',  ( -10.20829729246298712, 382.8698905601784759, -7.653668647301794969 ) ) ;
#19237 = AXIS2_PLACEMENT_3D ( 'NONE', #13029, #19620, #4798 ) ;
#19238 = DIRECTION ( 'NONE',  ( 0.000000000000000000, 0.000000000000000000, 1.000000000000000000 ) ) ;
#19239 = VERTEX_POINT ( 'NONE', #6547 ) ;
#19240 = ORIENTED_EDGE ( 'NONE', *, *, #5382, .F. ) ;
#19241 = CARTESIAN_POINT ( 'NONE',  ( -35.09675569278797269, 507.2448905683719431, 15.47720386886985366 ) ) ;
#19242 = CARTESIAN_POINT ( 'NONE',  ( -11.73070664223723902, 296.0573905765655809, 11.32908994701042005 ) ) ;
#19243 = ORIENTED_EDGE ( 'NONE', *, *, #12350, .F. ) ;
#19244 =( BOUNDED_CURVE ( )  B_SPLINE_CURVE ( 2, ( #1246, #9455, #20713, #21031, #20603, #18976, #19406, #12709, #7608, #14127, #19197, #14238, #9343, #15646, #17365, #5887, #11070 ),
 .UNSPECIFIED., .F., .T. ) 
 B_SPLINE_CURVE_WITH_KNOTS ( ( 3, 2, 2, 2, 2, 2, 2, 2, 3 ),
 ( 0.7812500000000001110, 0.7832031250000001110, 0.7851562500000001110, 0.7871093750000001110, 0.7890625000000002220, 0.7910156250000002220, 0.7929687500000002220, 0.7949218750000002220, 0.7968750000000002220 ),
 .UNSPECIFIED. ) 
 CURVE ( )  GEOMETRIC_REPRESENTATION_ITEM ( )  RATIONAL_B_SPLINE_CURVE ( ( 0.9999999999999988898, 0.9807852804032315408, 1.000000000000000000, 0.9807852804032304306, 1.000000000000000000, 0.9807852804032304306, 1.000000000000000000, 0.9807852804032304306, 1.000000000000000000, 0.9807852804032304306, 1.000000000000000000, 0.9807852804032304306, 1.000000000000000000, 0.9807852804032304306, 1.000000000000000000, 0.9807852804032282101, 1.000000000000002220 ) ) 
 REPRESENTATION_ITEM ( '' )  );
#19245 = CARTESIAN_POINT ( 'NONE',  ( -42.88789093042842637, 296.3073905683720000, 9.489475012073734561 ) ) ;
#19246 = CARTESIAN_POINT ( 'NONE',  ( -44.16309181155856578, 323.2448905683720000, -6.410867750099231266 ) ) ;
#19247 = VECTOR ( 'NONE', #17260, 1000.000000000000000 ) ;
#19248 = CARTESIAN_POINT ( 'NONE',  ( -40.01497788969913216, 270.4323905765655809, -16.95518130045146421 ) ) ;
#19249 = CARTESIAN_POINT ( 'NONE',  ( -47.16347859291445133, 396.6198905601784759, -7.653668647301793193 ) ) ;
#19250 = CARTESIAN_POINT ( 'NONE',  ( -28.68588794268870146, 241.3698905683720568, -16.75240474999999307 ) ) ;
#19251 = CARTESIAN_POINT ( 'NONE',  ( -42.88789093042844058, 396.3073905683719431, 9.489475012073736337 ) ) ;
#19252 = CIRCLE ( 'NONE', #17869, 20.00000000000000000 ) ;
#19253 = CYLINDRICAL_SURFACE ( 'NONE', #4405, 19.99999999999999645 ) ;
#19254 = DIRECTION ( 'NONE',  ( -0.000000000000000000, 1.000000000000000000, 1.155626614413199331E-16 ) ) ;
#19255 = PRODUCT ( 'Ram Linear Way Guides', 'Ram Linear Way Guides', '', ( #16597 ) ) ;
#19256 = CARTESIAN_POINT ( 'NONE',  ( -21.03221929538694113, 508.8698905765656377, -18.47759065022572855 ) ) ;
#19257 = CARTESIAN_POINT ( 'NONE',  ( -35.09675569278795138, 441.9948905683720568, -15.47720386886985544 ) ) ;
#19258 = ORIENTED_EDGE ( 'NONE', *, *, #992, .T. ) ;
#19259 = CARTESIAN_POINT ( 'NONE',  ( -48.68588794268871567, 447.2448905601785327, 0.000000000000000000 ) ) ;
#19260 = ADVANCED_FACE ( 'NONE', ( #89 ), #6656, .F. ) ;
#19261 = VERTEX_POINT ( 'NONE', #13165 ) ;
#19262 = VERTEX_POINT ( 'NONE', #3530 ) ;
#19263 = ORIENTED_EDGE ( 'NONE', *, *, #14132, .T. ) ;
#19264 = DIRECTION ( 'NONE',  ( -1.191790137725560488E-16, 1.000000000000000000, 0.000000000000000000 ) ) ;
#19265 = CARTESIAN_POINT ( 'NONE',  ( -10.20829729246298179, 331.6198905601784759, 7.653668647301790529 ) ) ;
#19266 = EDGE_CURVE ( 'NONE', #9807, #13610, #10118, .T. ) ;
#19267 = EDGE_CURVE ( 'NONE', #15984, #13902, #20186, .T. ) ;
#19268 = CARTESIAN_POINT ( 'NONE',  ( -32.01814843081344719, 367.5573905683721136, 16.75240474999999307 ) ) ;
#19269 = CARTESIAN_POINT ( 'NONE',  ( 0.2573354458087876995, -6.889406814520521394, 1.067197363239227537 ) ) ;
#19270 = CARTESIAN_POINT ( 'NONE',  ( -48.68588794268872277, 501.9948905765656377, 0.000000000000000000 ) ) ;
#19271 = CARTESIAN_POINT ( 'NONE',  ( -16.84014894278199392, 390.1198905683720000, -11.84573899990672707 ) ) ;
#19272 = CARTESIAN_POINT ( 'NONE',  ( -28.68588794268870146, 242.8698905683720568, -16.75240474999999307 ) ) ;
#19273 = CARTESIAN_POINT ( 'NONE',  ( -16.84014894278199037, 397.6198905683720568, 11.84573899990672530 ) ) ;
#19274 = CARTESIAN_POINT ( 'NONE',  ( -8.685887942688717445, 326.6823905765656377, 3.978247347593161010 ) ) ;
#19275 = CARTESIAN_POINT ( 'NONE',  ( 146.3141120573112630, 610.7448905601785327, 0.000000000000000000 ) ) ;
#19276 = CARTESIAN_POINT ( 'NONE',  ( -11.93348319268871549, 308.8698905683720000, -2.051577885510841163E-15 ) ) ;
#19277 = CARTESIAN_POINT ( 'NONE',  ( -38.17536295476246266, 466.9323905683720568, 14.20200298773971781 ) ) ;
#19278 = EDGE_CURVE ( 'NONE', #20328, #18325, #11955, .T. ) ;
#19279 = CARTESIAN_POINT ( 'NONE',  ( -32.66413529028188378, 459.4323905601785327, 19.99999999999999289 ) ) ;
#19280 = CARTESIAN_POINT ( 'NONE',  ( -48.68588794268870856, 367.2448905601784759, 0.000000000000000000 ) ) ;
#19281 = CARTESIAN_POINT ( 'NONE',  ( 0.5805565836007611225, 3.752776749732563033, 6.500000000000000000 ) ) ;
#19282 = CARTESIAN_POINT ( 'NONE',  ( -45.43829269268870519, 365.6823905683720568, 3.332260488124734632 ) ) ;
#19283 = CARTESIAN_POINT ( 'NONE',  ( -35.09675569278797269, 505.7448905683720000, 15.47720386886985366 ) ) ;
#19284 = CARTESIAN_POINT ( 'NONE',  ( -48.68588794268872277, 497.5573905601785327, 3.978247347593168115 ) ) ;
#19285 = CARTESIAN_POINT ( 'NONE',  ( -32.01814843081344009, 326.0573905683720000, 16.75240474999999307 ) ) ;
#19286 = ORIENTED_EDGE ( 'NONE', *, *, #4522, .F. ) ;
#19287 = CARTESIAN_POINT ( 'NONE',  ( -32.66413529028185536, 259.4323905601784190, 19.99999999999999289 ) ) ;
#19288 = ORIENTED_EDGE ( 'NONE', *, *, #18214, .T. ) ;
#19289 = CARTESIAN_POINT ( 'NONE',  ( -22.62331590640576451, 326.0737056351150613, 11.80838889663595914 ) ) ;
#19290 = AXIS2_PLACEMENT_3D ( 'NONE', #8059, #9898, #13276 ) ;
#19291 = CARTESIAN_POINT ( 'NONE',  ( -16.84014894278199392, 419.1198905683720000, 11.84573899990672530 ) ) ;
#19292 = DIRECTION ( 'NONE',  ( -1.000000000000000000, -0.000000000000000000, -0.000000000000000000 ) ) ;
#19293 = CYLINDRICAL_SURFACE ( 'NONE', #15252, 59.93977357075245038 ) ;
#19294 = CARTESIAN_POINT ( 'NONE',  ( -22.27502019258949773, 450.7448905683720000, -15.47720386886985544 ) ) ;
#19295 = B_SPLINE_CURVE_WITH_KNOTS ( 'NONE', 3,
 ( #14267, #8942, #14049, #17183, #4410, #18786, #10991, #10777, #967, #19120, #19225, #640, #14157, #12634, #7531, #15456, #9050, #6024, #17394, #17600, #8836, #5697, #7206, #3970 ),
 .UNSPECIFIED., .F., .F.,
 ( 4, 2, 2, 2, 2, 2, 2, 2, 2, 2, 2, 4 ),
 ( 0.000000000000000000, 0.002718680586849495009, 0.005437361173698990018, 0.006796701467123738606, 0.008156041760548486327, 0.01087472234739798004, 0.01223406264082271995, 0.01359340293424745640, 0.01631208352109693796, 0.01903076410794641779, 0.02039010440137115424, 0.02174944469479589415 ),
 .UNSPECIFIED. ) ;
#19296 = ORIENTED_EDGE ( 'NONE', *, *, #14271, .F. ) ;
#19297 = CARTESIAN_POINT ( 'NONE',  ( -16.84014894278200103, 460.1198905683720568, -11.84573899990672707 ) ) ;
#19298 = DIRECTION ( 'NONE',  ( 0.000000000000000000, 0.000000000000000000, 1.000000000000000000 ) ) ;
#19299 = LINE ( 'NONE', #14549, #2063 ) ;
#19300 = CARTESIAN_POINT ( 'NONE',  ( -45.64106924314018698, 381.0573905765656377, -11.32908994701042715 ) ) ;
#19301 = DIRECTION ( 'NONE',  ( -0.3512089204514986518, 0.000000000000000000, 0.9362971185447986899 ) ) ;
#19302 = CARTESIAN_POINT ( 'NONE',  ( -45.64106924314017988, 371.0573905765656946, -11.32908994701042538 ) ) ;
#19303 = LINE ( 'NONE', #20715, #6000 ) ;
#19304 = CARTESIAN_POINT ( 'NONE',  ( -10.76731745429010090, 56.85652257517428865, -152.3753892284480003 ) ) ;
#19305 = PLANE ( 'NONE',  #1994 ) ;
#19306 = LINE ( 'NONE', #13030, #4872 ) ;
#19307 = CARTESIAN_POINT ( 'NONE',  ( -42.82802356641965957, 345.9948905601784759, -14.14213562373094746 ) ) ;
#19308 = CARTESIAN_POINT ( 'NONE',  ( -11.93348319268872793, 420.0573905683720000, 3.332260488124728415 ) ) ;
#19309 = DIRECTION ( 'NONE',  ( -1.191790137725560488E-16, 1.000000000000000000, 0.000000000000000000 ) ) ;
#19310 = CARTESIAN_POINT ( 'NONE',  ( -32.01814843081343298, 247.5573905683720000, 16.75240474999999307 ) ) ;
#19311 = VERTEX_POINT ( 'NONE', #10431 ) ;
#19312 = CARTESIAN_POINT ( 'NONE',  ( -36.33955658999052218, 423.8698905765655809, 18.47759065022572500 ) ) ;
#19313 = ORIENTED_EDGE ( 'NONE', *, *, #15061, .T. ) ;
#19314 = CARTESIAN_POINT ( 'NONE',  ( -38.17536295476246977, 463.8073905683720000, -14.20200298773971426 ) ) ;
#19315 = CARTESIAN_POINT ( 'NONE',  ( -10.20829729246297291, 236.3698905765656093, 7.653668647301790529 ) ) ;
#19316 = EDGE_CURVE ( 'NONE', #289, #5907, #8054, .T. ) ;
#19317 = EDGE_LOOP ( 'NONE', ( #19629, #151, #19792 ) ) ;
#19318 = CARTESIAN_POINT ( 'NONE',  ( 65.85920792673738333, 160.1716627696692683, -20.00000000000000355 ) ) ;
#19319 = CARTESIAN_POINT ( 'NONE',  ( -11.93348319268870661, 229.1823905683720284, -3.332260488124732856 ) ) ;
#19320 = EDGE_LOOP ( 'NONE', ( #2779, #18568 ) ) ;
#19321 = CARTESIAN_POINT ( 'NONE',  ( -19.19641293061500065, 527.3073905683720568, 14.20200298773971426 ) ) ;
#19322 = LINE ( 'NONE', #2897, #399 ) ;
#19323 = VECTOR ( 'NONE', #14525, 1000.000000000000000 ) ;
#19324 = CARTESIAN_POINT ( 'NONE',  ( -14.54375231895778242, 458.2448905765656377, -14.14213562373094746 ) ) ;
#19325 = CARTESIAN_POINT ( 'NONE',  ( 20.42502041961813930, 230.5765313837437418, -40.00000000000000000 ) ) ;
#19326 = EDGE_CURVE ( 'NONE', #6197, #5267, #8401, .T. ) ;
#19327 = DIRECTION ( 'NONE',  ( -1.191790137725560488E-16, 1.000000000000000000, -0.000000000000000000 ) ) ;
#19328 = CARTESIAN_POINT ( 'NONE',  ( -48.68588794268860198, 241.6823905765656093, -3.978247347593371508 ) ) ;
#19329 = DIRECTION ( 'NONE',  ( 1.000000000000000000, 0.000000000000000000, 0.000000000000000000 ) ) ;
#19330 = CARTESIAN_POINT ( 'NONE',  ( -8.685887942688703234, 223.9102039777117454, 1.614530918564491380 ) ) ;
#19331 = CARTESIAN_POINT ( 'NONE',  ( -44.16309181155855157, 234.4948905683720284, 6.410867750099241924 ) ) ;
#19332 = CARTESIAN_POINT ( 'NONE',  ( -11.93348319268871727, 320.0573905683720000, 3.332260488124728415 ) ) ;
#19333 = CARTESIAN_POINT ( 'NONE',  ( -14.54375231895778064, 443.4948905601784759, -14.14213562373094746 ) ) ;
#19334 = CARTESIAN_POINT ( 'NONE',  ( 5.674999999999999822, 4.898587196589412829E-16, -4.000000000000000000 ) ) ;
#19335 = B_SPLINE_CURVE_WITH_KNOTS ( 'NONE', 1,
 ( #3273, #9848 ),
 .UNSPECIFIED., .F., .F.,
 ( 2, 2 ),
 ( 0.000000000000000000, 1.000000000000000000 ),
 .UNSPECIFIED. ) ;
#19336 = CARTESIAN_POINT ( 'NONE',  ( -13.20868407381885312, 300.9948905683720568, -6.410867750099233042 ) ) ;
#19337 = CARTESIAN_POINT ( 'NONE',  ( -14.48388495494900141, 387.9323905683720000, 9.489475012073732785 ) ) ;
#19338 = CARTESIAN_POINT ( 'NONE',  ( -28.68588794268873698, 532.8698905683719431, -16.75240474999999307 ) ) ;
#19339 = CARTESIAN_POINT ( 'NONE',  ( -47.16347859291444422, 376.6198905601784759, -7.653668647301793193 ) ) ;
#19340 = ADVANCED_FACE ( 'NONE', ( #15220 ), #20291, .T. ) ;
#19341 = CARTESIAN_POINT ( 'NONE',  ( -45.64106924314018698, 406.3073905601785327, -11.32908994701042538 ) ) ;
#19342 = EDGE_LOOP ( 'NONE', ( #20174, #20813, #19522, #20995 ) ) ;
#19343 = ORIENTED_EDGE ( 'NONE', *, *, #15923, .F. ) ;
#19344 = CARTESIAN_POINT ( 'NONE',  ( -16.84014894278200103, 489.1198905683720000, 11.84573899990672530 ) ) ;
#19345 = CARTESIAN_POINT ( 'NONE',  ( 5.674999999999999822, 0.000000000000000000, 0.000000000000000000 ) ) ;
#19346 = EDGE_LOOP ( 'NONE', ( #16875, #18004, #21339, #7308 ) ) ;
#19347 = CARTESIAN_POINT ( 'NONE',  ( -35.09675569278793716, 293.4948905683720000, -15.47720386886985544 ) ) ;
#19348 = CARTESIAN_POINT ( 'NONE',  ( -45.43829269268869808, 323.5573905683720000, -3.332260488124726194 ) ) ;
#19349 = CARTESIAN_POINT ( 'NONE',  ( -48.68588794268869435, 262.3073905765655809, 3.978247347593168115 ) ) ;
#19350 = AXIS2_PLACEMENT_3D ( 'NONE', #9450, #2973, #14660 ) ;
#19351 = DIRECTION ( 'NONE',  ( -0.8865057725575725689, 0.000000000000000000, 0.4627175328665443232 ) ) ;
#19352 = CARTESIAN_POINT ( 'NONE',  ( 166.1493775951145437, 610.7448905601785327, 8.917803138848105604 ) ) ;
#19353 = CARTESIAN_POINT ( 'NONE',  ( -19.19641293061498999, 381.9323905683720568, -14.20200298773971603 ) ) ;
#19354 = EDGE_CURVE ( 'NONE', #19427, #21369, #12091, .T. ) ;
#19355 = DIRECTION ( 'NONE',  ( 0.1337298367054296222, -0.9910178256594273094, 0.000000000000000000 ) ) ;
#19356 = CIRCLE ( 'NONE', #15925, 5.000000000000004441 ) ;
#19357 = LINE ( 'NONE', #9297, #12113 ) ;
#19358 = CARTESIAN_POINT ( 'NONE',  ( -45.64106924314020119, 511.0573905765657514, -11.32908994701042538 ) ) ;
#19359 = CARTESIAN_POINT ( 'NONE',  ( -28.68588794268872277, 446.3698905683720000, 16.75240474999999307 ) ) ;
#19360 = DIRECTION ( 'NONE',  ( 0.000000000000000000, 1.000000000000000000, 0.000000000000000000 ) ) ;
#19361 = VERTEX_POINT ( 'NONE', #13489 ) ;
#19362 =( BOUNDED_CURVE ( )  B_SPLINE_CURVE ( 2, ( #5385, #3666, #16873, #15046, #119, #6693, #5283, #5495, #7113, #13738, #441, #3564, #9934, #13524, #2057, #15153, #8630 ),
 .UNSPECIFIED., .F., .T. ) 
 B_SPLINE_CURVE_WITH_KNOTS ( ( 3, 2, 2, 2, 2, 2, 2, 2, 3 ),
 ( 0.07812500000000043021, 0.08007812500000038858, 0.08203125000000034694, 0.08398437500000030531, 0.08593750000000024980, 0.08789062500000020817, 0.08984375000000016653, 0.09179687500000012490, 0.09375000000000008327 ),
 .UNSPECIFIED. ) 
 CURVE ( )  GEOMETRIC_REPRESENTATION_ITEM ( )  RATIONAL_B_SPLINE_CURVE ( ( 0.9999999999999957812, 0.9807852804032346494, 1.000000000000000000, 0.9807852804032304306, 1.000000000000000000, 0.9807852804032304306, 1.000000000000000000, 0.9807852804032304306, 1.000000000000000000, 0.9807852804032304306, 1.000000000000000000, 0.9807852804032304306, 1.000000000000000000, 0.9807852804032304306, 1.000000000000000000, 0.9807852804032296534, 1.000000000000000888 ) ) 
 REPRESENTATION_ITEM ( '' )  );
#19363 = CARTESIAN_POINT ( 'NONE',  ( -36.33955658999052218, 455.3698905601784759, -18.47759065022572855 ) ) ;
#19364 = ADVANCED_FACE ( 'NONE', ( #8918 ), #2235, .T. ) ;
#19365 = ORIENTED_EDGE ( 'NONE', *, *, #9348, .F. ) ;
#19366 = AXIS2_PLACEMENT_3D ( 'NONE', #12919, #19508, #4686 ) ;
#19367 = ORIENTED_EDGE ( 'NONE', *, *, #21219, .F. ) ;
#19368 = ORIENTED_EDGE ( 'NONE', *, *, #19009, .F. ) ;
#19369 = CARTESIAN_POINT ( 'NONE',  ( -11.73070664223724613, 356.0573905765655809, 11.32908994701042005 ) ) ;
#19370 = CARTESIAN_POINT ( 'NONE',  ( -14.54375231895776643, 333.4948905601784759, -14.14213562373094746 ) ) ;
#19371 = CARTESIAN_POINT ( 'NONE',  ( -45.20498122175430922, 223.9102039777117739, -2.861862797699382011 ) ) ;
#19372 = CARTESIAN_POINT ( 'NONE',  ( -38.17536295476245556, 363.8073905683720000, -14.20200298773971426 ) ) ;
#19373 = CARTESIAN_POINT ( 'NONE',  ( 29.72350413846044859, 280.4463447002762564, -40.00000000000000000 ) ) ;
#19374 = VECTOR ( 'NONE', #1446, 1000.000000000000000 ) ;
#19375 = CARTESIAN_POINT ( 'NONE',  ( -47.16347859291446554, 511.3698905765655809, -7.653668647301793193 ) ) ;
#19376 = CARTESIAN_POINT ( 'NONE',  ( -42.88789093042843348, 384.8073905683720000, 9.489475012073736337 ) ) ;
#19377 = CARTESIAN_POINT ( 'NONE',  ( -22.27502019258946930, 222.2448905683720568, -15.47720386886985544 ) ) ;
#19378 = CARTESIAN_POINT ( 'NONE',  ( -44.16309181155857289, 383.2448905683720000, -6.410867750099231266 ) ) ;
#19379 = CARTESIAN_POINT ( 'NONE',  ( -24.70764059509555821, 319.1823905765655809, -19.99999999999999289 ) ) ;
#19380 = CARTESIAN_POINT ( 'NONE',  ( -17.35679799567830273, 423.8073905601785327, -16.95518130045146421 ) ) ;
#19381 = CARTESIAN_POINT ( 'NONE',  ( -22.27502019258946930, 286.9948905683720000, 15.47720386886985189 ) ) ;
#19382 = CARTESIAN_POINT ( 'NONE',  ( -44.16309181155858710, 454.7448905683720568, -6.410867750099231266 ) ) ;
#19383 = CARTESIAN_POINT ( 'NONE',  ( -21.03221929538691981, 460.3698905601784759, 18.47759065022572500 ) ) ;
#19384 = CARTESIAN_POINT ( 'NONE',  ( 51.50493485826542184, 141.8799693780962912, -20.00000000000000355 ) ) ;
#19385 = LINE ( 'NONE', #4136, #8142 ) ;
#19386 = CIRCLE ( 'NONE', #758, 15.00000000000000000 ) ;
#19387 = CARTESIAN_POINT ( 'NONE',  ( -11.93348319268872260, 370.0573905683719431, 3.332260488124728415 ) ) ;
#19388 = CARTESIAN_POINT ( 'NONE',  ( -25.35362745456399836, 506.6823905683720568, 16.75240474999998952 ) ) ;
#19389 = CARTESIAN_POINT ( 'NONE',  ( -11.73070664223726389, 501.3073905601785327, 11.32908994701042005 ) ) ;
#19390 = CARTESIAN_POINT ( 'NONE',  ( -44.16309181155857289, 333.2448905683720568, -6.410867750099231266 ) ) ;
#19391 = ORIENTED_EDGE ( 'NONE', *, *, #5373, .F. ) ;
#19392 = CARTESIAN_POINT ( 'NONE',  ( -17.35679799567827786, 260.6823905601785327, 16.95518130045146421 ) ) ;
#19393 = ORIENTED_EDGE ( 'NONE', *, *, #7494, .F. ) ;
#19394 = EDGE_CURVE ( 'NONE', #13316, #10104, #20394, .T. ) ;
#19395 = CARTESIAN_POINT ( 'NONE',  ( -8.685887942688742314, 573.2448905601785327, 2.449293598294706119E-15 ) ) ;
#19396 = EDGE_CURVE ( 'NONE', #1687, #17091, #11537, .T. ) ;
#19397 = CARTESIAN_POINT ( 'NONE',  ( -32.01814843081344719, 427.5573905683720568, 16.75240474999999307 ) ) ;
#19398 = CARTESIAN_POINT ( 'NONE',  ( -48.68588794268871567, 391.9948905765656377, 0.000000000000000000 ) ) ;
#19399 = CARTESIAN_POINT ( 'NONE',  ( -28.68588794268874054, 573.2448905601785327, 0.000000000000000000 ) ) ;
#19400 = CARTESIAN_POINT ( 'NONE',  ( -32.01814843081346140, 451.6823905683720568, -16.75240474999999307 ) ) ;
#19401 = ORIENTED_EDGE ( 'NONE', *, *, #5957, .F. ) ;
#19402 = CARTESIAN_POINT ( 'NONE',  ( -25.35362745456400546, 471.0573905683721136, -16.75240474999999307 ) ) ;
#19403 = DIRECTION ( 'NONE',  ( 0.000000000000000000, -1.000000000000000000, 0.000000000000000000 ) ) ;
#19404 = DIRECTION ( 'NONE',  ( 1.000000000000000000, 0.000000000000000000, -3.836511174089486666E-16 ) ) ;
#19405 = CARTESIAN_POINT ( 'NONE',  ( -14.54375231895777176, 378.2448905765656377, -14.14213562373094746 ) ) ;
#19406 = CARTESIAN_POINT ( 'NONE',  ( -36.33955658999050087, 280.1198905765656377, -18.47759065022572855 ) ) ;
#19407 = CIRCLE ( 'NONE', #6272, 59.93977357075245038 ) ;
#19408 = CARTESIAN_POINT ( 'NONE',  ( -11.73070664223724968, 367.9323905765655809, -11.32908994701042538 ) ) ;
#19409 = DIRECTION ( 'NONE',  ( 1.000000000000000000, 0.000000000000000000, 0.000000000000000000 ) ) ;
#19410 = CARTESIAN_POINT ( 'NONE',  ( -45.64106924314016567, 252.9323905765656377, 11.32908994701042538 ) ) ;
#19411 = VECTOR ( 'NONE', #305, 1000.000000000000000 ) ;
#19412 = LINE ( 'NONE', #9245, #3687 ) ;
#19413 = CARTESIAN_POINT ( 'NONE',  ( -11.73070664223724791, 343.1823905601785327, -11.32908994701042538 ) ) ;
#19414 = CARTESIAN_POINT ( 'NONE',  ( -14.48388495494900496, 421.3073905683720000, -9.489475012073736337 ) ) ;
#19415 = DIRECTION ( 'NONE',  ( 1.000000000000000000, 1.250996701150283068E-16, -0.000000000000000000 ) ) ;
#19416 = CARTESIAN_POINT ( 'NONE',  ( -42.88789093042841927, 254.4323905683720284, -9.489475012073736337 ) ) ;
#19417 = ORIENTED_EDGE ( 'NONE', *, *, #12595, .T. ) ;
#19418 = VERTEX_POINT ( 'NONE', #4055 ) ;
#19419 = DIRECTION ( 'NONE',  ( 0.000000000000000000, 0.000000000000000000, -1.000000000000000000 ) ) ;
#19420 = ORIENTED_EDGE ( 'NONE', *, *, #1523, .F. ) ;
#19421 = CARTESIAN_POINT ( 'NONE',  ( -25.35362745456399125, 458.1823905683719431, 16.75240474999998952 ) ) ;
#19422 = AXIS2_PLACEMENT_3D ( 'NONE', #10822, #2615, #7784 ) ;
#19423 = CARTESIAN_POINT ( 'NONE',  ( -42.82802356641964536, 220.7448905765656093, -14.14213562373094746 ) ) ;
#19424 = ORIENTED_EDGE ( 'NONE', *, *, #9858, .F. ) ;
#19425 = CARTESIAN_POINT ( 'NONE',  ( -42.88446638378037790, 206.4484180351193174, 4.837872587287140647 ) ) ;
#19426 = CARTESIAN_POINT ( 'NONE',  ( -16.84014894278201169, 531.6198905683720568, -11.84573899990672707 ) ) ;
#19427 = VERTEX_POINT ( 'NONE', #10643 ) ;
#19428 = DIRECTION ( 'NONE',  ( 0.000000000000000000, 0.000000000000000000, 1.000000000000000000 ) ) ;
#19429 = CARTESIAN_POINT ( 'NONE',  ( 60.03793209889851568, 30.52886280891152282, -131.1729372809869005 ) ) ;
#19430 = CARTESIAN_POINT ( 'NONE',  ( -11.73070664223725501, 436.0573905765656377, 11.32908994701042005 ) ) ;
#19431 = PRODUCT ( 'Flywheel Manual Operating Handles', 'Flywheel Manual Operating Handles', '', ( #7051 ) ) ;
#19432 = CARTESIAN_POINT ( 'NONE',  ( -47.16347859291444422, 347.8698905601784759, 7.653668647301805628 ) ) ;
#19433 = DIRECTION ( 'NONE',  ( -0.6352526299242171604, 0.000000000000000000, -0.7723044064191046942 ) ) ;
#19434 = CARTESIAN_POINT ( 'NONE',  ( -48.68588794268869435, 241.9948905765656377, 0.000000000000000000 ) ) ;
#19435 = CARTESIAN_POINT ( 'NONE',  ( -48.68588794268870146, 271.9948905765656377, 0.000000000000000000 ) ) ;
#19436 = AXIS2_PLACEMENT_3D ( 'NONE', #18236, #13490, #8388 ) ;
#19437 = LINE ( 'NONE', #4620, #21142 ) ;
#19438 = FACE_BOUND ( 'NONE', #7064, .T. ) ;
#19439 = CARTESIAN_POINT ( 'NONE',  ( -13.20868407381885490, 320.9948905683720568, -6.410867750099233042 ) ) ;
#19440 = CARTESIAN_POINT ( 'NONE',  ( -42.82802356641964536, 235.9948905601784759, -14.14213562373094746 ) ) ;
#19441 = CARTESIAN_POINT ( 'NONE',  ( -1.025382690249031503, 135.1716627696692683, -25.00000000000000000 ) ) ;
#19442 = CARTESIAN_POINT ( 'NONE',  ( -44.16309181155856578, 314.7448905683720000, -6.410867750099231266 ) ) ;
#19443 = CARTESIAN_POINT ( 'NONE',  ( -32.01814843081344719, 371.6823905683720000, -16.75240474999999307 ) ) ;
#19444 = EDGE_CURVE ( 'NONE', #21047, #14199, #9877, .T. ) ;
#19445 = CARTESIAN_POINT ( 'NONE',  ( -38.17536295476247687, 533.8073905683720568, -14.20200298773971426 ) ) ;
#19446 = CIRCLE ( 'NONE', #117, 4.000000000000003553 ) ;
#19447 = CARTESIAN_POINT ( 'NONE',  ( -11.73070664223725146, 373.1823905601784759, -11.32908994701042715 ) ) ;
#19448 = CARTESIAN_POINT ( 'NONE',  ( -28.68588794268871922, 404.7448905601784759, -19.99999999999999289 ) ) ;
#19449 = ORIENTED_EDGE ( 'NONE', *, *, #13664, .F. ) ;
#19450 = CARTESIAN_POINT ( 'NONE',  ( -22.27502019258949062, 488.4948905683720568, 15.47720386886985189 ) ) ;
#19451 = CYLINDRICAL_SURFACE ( 'NONE', #11445, 19.99999999999999645 ) ;
#19452 = CARTESIAN_POINT ( 'NONE',  ( -16.84014894278197971, 287.6198905683720000, 11.84573899990672530 ) ) ;
#19453 = VERTEX_POINT ( 'NONE', #11073 ) ;
#19454 = CARTESIAN_POINT ( 'NONE',  ( -11.93348319268871016, 280.0573905683720568, 3.332260488124728859 ) ) ;
#19455 = CARTESIAN_POINT ( 'NONE',  ( -28.68588794268870856, 316.3698905683720568, 16.75240474999999307 ) ) ;
#19456 = CARTESIAN_POINT ( 'NONE',  ( -25.35362745456398059, 262.5573905683720000, -16.75240474999999307 ) ) ;
#19457 = AXIS2_PLACEMENT_3D ( 'NONE', #5079, #11458, #4865 ) ;
#19458 = CARTESIAN_POINT ( 'NONE',  ( -40.01497788969911795, 263.5573905765656377, 16.95518130045146776 ) ) ;
#19459 = DIRECTION ( 'NONE',  ( -1.000000000000000000, 0.000000000000000000, 0.000000000000000000 ) ) ;
#19460 = CARTESIAN_POINT ( 'NONE',  ( -11.93348319268870661, 228.5573905683720568, 3.332260488124728859 ) ) ;
#19461 = CIRCLE ( 'NONE', #20864, 6.500000000000000888 ) ;
#19462 = CARTESIAN_POINT ( 'NONE',  ( -25.35362745456399125, 372.5573905683720568, -16.75240474999999307 ) ) ;
#19463 = ADVANCED_FACE ( 'NONE', ( #12608 ), #6204, .F. ) ;
#19464 = PLANE ( 'NONE',  #9914 ) ;
#19465 = DIRECTION ( 'NONE',  ( 1.191790137725560488E-16, -1.000000000000000000, -0.000000000000000000 ) ) ;
#19466 = DIRECTION ( 'NONE',  ( 0.000000000000000000, -1.000000000000000000, 0.000000000000000000 ) ) ;
#19467 = CARTESIAN_POINT ( 'NONE',  ( -16.84014894278199748, 437.6198905683720000, 11.84573899990672530 ) ) ;
#19468 = DIRECTION ( 'NONE',  ( -0.3090169943749475068, 0.000000000000000000, -0.9510565162951535312 ) ) ;
#19469 = ORIENTED_EDGE ( 'NONE', *, *, #2364, .T. ) ;
#19470 = CARTESIAN_POINT ( 'NONE',  ( -36.33955658999051508, 425.3698905601784759, -18.47759065022572855 ) ) ;
#19471 = VECTOR ( 'NONE', #18854, 1000.000000000000114 ) ;
#19472 = VERTEX_POINT ( 'NONE', #17367 ) ;
#19473 = ORIENTED_EDGE ( 'NONE', *, *, #20691, .F. ) ;
#19474 = EDGE_LOOP ( 'NONE', ( #4578, #9940, #9776, #3334 ) ) ;
#19475 = DIRECTION ( 'NONE',  ( -1.000000000000000000, -1.191790137725560488E-16, 0.000000000000000000 ) ) ;
#19476 = CARTESIAN_POINT ( 'NONE',  ( -11.73070664223723902, 311.3073905601784759, 11.32908994701042005 ) ) ;
#19477 = DIRECTION ( 'NONE',  ( -1.000000000000000000, 0.000000000000000000, 0.000000000000000000 ) ) ;
#19478 = AXIS2_PLACEMENT_3D ( 'NONE', #8389, #19974, #11750 ) ;
#19479 = EDGE_CURVE ( 'NONE', #2963, #12191, #17574, .T. ) ;
#19480 = CARTESIAN_POINT ( 'NONE',  ( -16.84014894278198682, 341.6198905683720000, -11.84573899990672707 ) ) ;
#19481 = CARTESIAN_POINT ( 'NONE',  ( -28.68588794268873343, 499.4948905765656377, -19.99999999999999289 ) ) ;
#19482 = CARTESIAN_POINT ( 'NONE',  ( -16.84014894278199037, 377.6198905683720568, 11.84573899990672530 ) ) ;
#19483 = CARTESIAN_POINT ( 'NONE',  ( 35.96497763894178945, 230.5765313837437418, -60.00000000000000000 ) ) ;
#19484 = CARTESIAN_POINT ( 'NONE',  ( -35.09675569278795138, 385.7448905683720000, 15.47720386886985366 ) ) ;
#19485 = CARTESIAN_POINT ( 'NONE',  ( -10.20829729246298001, 316.3698905765656377, 7.653668647301790529 ) ) ;
#19486 = CARTESIAN_POINT ( 'NONE',  ( -10.20829729246299244, 422.8698905601784759, -7.653668647301794969 ) ) ;
#19487 = CARTESIAN_POINT ( 'NONE',  ( -19.19641293061497578, 290.4323905683720568, -14.20200298773971603 ) ) ;
#19488 =( NAMED_UNIT ( * ) SI_UNIT ( $, .STERADIAN. ) SOLID_ANGLE_UNIT ( ) );
#19489 = CARTESIAN_POINT ( 'NONE',  ( -45.43829269268871940, 445.3698905683720000, 0.000000000000000000 ) ) ;
#19490 = EDGE_CURVE ( 'NONE', #2298, #2858, #3242, .T. ) ;
#19491 = CARTESIAN_POINT ( 'NONE',  ( -24.70764059509554755, 284.4323905601784759, -19.99999999999999289 ) ) ;
#19492 = CARTESIAN_POINT ( 'NONE',  ( -8.685887942688724550, 372.2448905601784759, -2.449293598294705724E-15 ) ) ;
#19493 = DIRECTION ( 'NONE',  ( -1.191790137725560488E-16, 1.000000000000000000, -0.000000000000000000 ) ) ;
#19494 = CIRCLE ( 'NONE', #18792, 10.00000000000000178 ) ;
#19495 = CARTESIAN_POINT ( 'NONE',  ( -13.20868407381885667, 339.7448905683720568, 6.410867750099229490 ) ) ;
#19496 = CARTESIAN_POINT ( 'NONE',  ( -44.16309181155857999, 504.4948905683720568, 6.410867750099241924 ) ) ;
#19497 = CARTESIAN_POINT ( 'NONE',  ( -45.64106924314020119, 496.3073905601784759, -11.32908994701042715 ) ) ;
#19498 = CARTESIAN_POINT ( 'NONE',  ( -25.35362745456397704, 316.6823905683720000, 16.75240474999998952 ) ) ;
#19499 = ORIENTED_EDGE ( 'NONE', *, *, #12213, .F. ) ;
#19500 = CARTESIAN_POINT ( 'NONE',  ( -24.70764059509553334, 260.0573905601784759, 19.99999999999998934 ) ) ;
#19501 = ORIENTED_EDGE ( 'NONE', *, *, #20722, .T. ) ;
#19502 = DIRECTION ( 'NONE',  ( -0.000000000000000000, -0.000000000000000000, -1.000000000000000000 ) ) ;
#19503 = CARTESIAN_POINT ( 'NONE',  ( -32.01814843081344719, 403.1823905683720000, -16.75240474999999307 ) ) ;
#19504 = CARTESIAN_POINT ( 'NONE',  ( -31.26501780185373391, 205.1437886375728965, 0.000000000000000000 ) ) ;
#19505 = PRESENTATION_STYLE_ASSIGNMENT (( #21130 ) ) ;
#19506 = CARTESIAN_POINT ( 'NONE',  ( -19.19641293061499354, 440.4323905683720000, -14.20200298773971603 ) ) ;
#19507 = CARTESIAN_POINT ( 'NONE',  ( -42.88789093042844769, 452.9323905683721136, -9.489475012073734561 ) ) ;
#19508 = DIRECTION ( 'NONE',  ( -0.9647579637146499465, -0.2631388824350414657, 0.000000000000000000 ) ) ;
#19509 = CARTESIAN_POINT ( 'NONE',  ( -10.20829729246299067, 412.8698905601784759, -7.653668647301794969 ) ) ;
#19510 = CARTESIAN_POINT ( 'NONE',  ( -21.03221929538691271, 385.1198905765656377, 18.47759065022572500 ) ) ;
#19511 = CARTESIAN_POINT ( 'NONE',  ( -27.55128289072937875, 46.57285964785339161, 49.58849804005138395 ) ) ;
#19512 = FACE_BOUND ( 'NONE', #1143, .T. ) ;
#19513 = DIRECTION ( 'NONE',  ( -0.000000000000000000, -1.000000000000000000, -0.000000000000000000 ) ) ;
#19514 = DIRECTION ( 'NONE',  ( 0.000000000000000000, -1.000000000000000000, 0.000000000000000000 ) ) ;
#19515 = CARTESIAN_POINT ( 'NONE',  ( -40.53162694259545162, 496.6198905683720000, 11.84573899990672885 ) ) ;
#19516 = CARTESIAN_POINT ( 'NONE',  ( 51.98438129372387806, 30.52886280891151216, 94.99999999999994316 ) ) ;
#19517 = CARTESIAN_POINT ( 'NONE',  ( -13.68588794268869790, 213.9102039777116602, 1.836970198721029589E-15 ) ) ;
#19518 = CARTESIAN_POINT ( 'NONE',  ( -40.01497788969913927, 345.6823905601784759, -16.95518130045146421 ) ) ;
#19519 = CARTESIAN_POINT ( 'NONE',  ( -28.68588794268871922, 407.8698905683720568, 16.75240474999999307 ) ) ;
#19520 = CARTESIAN_POINT ( 'NONE',  ( 20.42502041961806825, 281.1055109169419666, 20.00000000000000355 ) ) ;
#19521 = CARTESIAN_POINT ( 'NONE',  ( -19.19641293061496867, 248.8073905683720284, 14.20200298773971426 ) ) ;
#19522 = ORIENTED_EDGE ( 'NONE', *, *, #5783, .F. ) ;
#19523 = VERTEX_POINT ( 'NONE', #14129 ) ;
#19524 = FACE_OUTER_BOUND ( 'NONE', #6903, .T. ) ;
#19525 = VERTEX_POINT ( 'NONE', #10752 ) ;
#19526 = CARTESIAN_POINT ( 'NONE',  ( -45.43829269268872650, 455.0573905683720000, -3.332260488124726638 ) ) ;
#19527 = CARTESIAN_POINT ( 'NONE',  ( -42.82802356641964536, 233.2448905765656093, 14.14213562373094923 ) ) ;
#19528 = EDGE_CURVE ( 'NONE', #20892, #12520, #4378, .T. ) ;
#19529 = EDGE_LOOP ( 'NONE', ( #7809, #14462, #8905, #5661 ) ) ;
#19530 = CARTESIAN_POINT ( 'NONE',  ( -43.37409492154782242, 209.1153864038857648, 3.054836571872670881 ) ) ;
#19531 = CARTESIAN_POINT ( 'NONE',  ( -14.48388495494901740, 529.4323905683720568, 9.489475012073732785 ) ) ;
#19532 = EDGE_CURVE ( 'NONE', #5342, #12984, #8170, .T. ) ;
#19533 = ORIENTED_EDGE ( 'NONE', *, *, #17501, .F. ) ;
#19534 = CARTESIAN_POINT ( 'NONE',  ( -45.43829269268872650, 504.1823905683721136, 3.332260488124734632 ) ) ;
#19535 = DIRECTION ( 'NONE',  ( 0.000000000000000000, 0.000000000000000000, 1.000000000000000000 ) ) ;
#19536 = EDGE_CURVE ( 'NONE', #2675, #12300, #9457, .T. ) ;
#19537 = CARTESIAN_POINT ( 'NONE',  ( -28.68588794268872277, 444.4948905765655809, 19.99999999999999289 ) ) ;
#19538 = CARTESIAN_POINT ( 'NONE',  ( -47.16347859291443712, 301.3698905765655809, -7.653668647301793193 ) ) ;
#19539 = CARTESIAN_POINT ( 'NONE',  ( -16.84014894278198327, 337.6198905683720000, 11.84573899990672530 ) ) ;
#19540 = DIRECTION ( 'NONE',  ( -1.000000000000000000, 0.000000000000000000, 0.000000000000000000 ) ) ;
#19541 = FACE_BOUND ( 'NONE', #1525, .T. ) ;
#19542 = CARTESIAN_POINT ( 'NONE',  ( -48.68588794268879383, 287.5573905601784759, 3.978247347592954952 ) ) ;
#19543 = CARTESIAN_POINT ( 'NONE',  ( -38.17536295476243424, 225.4323905683720000, 14.20200298773971781 ) ) ;
#19544 = CARTESIAN_POINT ( 'NONE',  ( -40.53162694259543031, 326.6198905683720568, 11.84573899990672885 ) ) ;
#19545 = EDGE_CURVE ( 'NONE', #19877, #19032, #19303, .T. ) ;
#19546 = PLANE ( 'NONE',  #4016 ) ;
#19547 = CARTESIAN_POINT ( 'NONE',  ( -25.35362745456397704, 318.1823905683720568, 16.75240474999998952 ) ) ;
#19548 = CARTESIAN_POINT ( 'NONE',  ( -38.17536295476246977, 516.9323905683720568, 14.20200298773971781 ) ) ;
#19549 =( BOUNDED_CURVE ( )  B_SPLINE_CURVE ( 2, ( #20614, #15549, #5578, #17060, #15438, #5683, #732, #625, #9249, #18987, #4065, #10649, #17375, #4168, #12289, #17268, #2452 ),
 .UNSPECIFIED., .F., .T. ) 
 B_SPLINE_CURVE_WITH_KNOTS ( ( 3, 2, 2, 2, 2, 2, 2, 2, 3 ),
 ( 0.3906250000000001665, 0.3925781250000001665, 0.3945312500000001665, 0.3964843750000001665, 0.3984375000000001665, 0.4003906250000001665, 0.4023437500000001665, 0.4042968750000001665, 0.4062500000000001665 ),
 .UNSPECIFIED. ) 
 CURVE ( )  GEOMETRIC_REPRESENTATION_ITEM ( )  RATIONAL_B_SPLINE_CURVE ( ( 0.9999999999999983347, 0.9807852804032320959, 1.000000000000000000, 0.9807852804032304306, 1.000000000000000000, 0.9807852804032304306, 1.000000000000000000, 0.9807852804032304306, 1.000000000000000000, 0.9807852804032304306, 1.000000000000000000, 0.9807852804032304306, 1.000000000000000000, 0.9807852804032304306, 1.000000000000000000, 0.9807852804032287652, 1.000000000000001554 ) ) 
 REPRESENTATION_ITEM ( '' )  );
#19550 = CARTESIAN_POINT ( 'NONE',  ( -8.685887942688722774, 372.5573905601784759, -3.978247347593165895 ) ) ;
#19551 = CARTESIAN_POINT ( 'NONE',  ( -24.70764059509554755, 229.1823905765656377, -19.99999999999999289 ) ) ;
#19552 = ORIENTED_EDGE ( 'NONE', *, *, #15044, .T. ) ;
#19553 = CARTESIAN_POINT ( 'NONE',  ( -11.93348319268873503, 480.6823905683720000, -3.332260488124732856 ) ) ;
#19554 = CARTESIAN_POINT ( 'NONE',  ( -28.68588794268874054, 573.2448905601785327, 0.000000000000000000 ) ) ;
#19555 = CARTESIAN_POINT ( 'NONE',  ( -11.93348319268871371, 279.1823905683720000, -3.332260488124732856 ) ) ;
#19556 = EDGE_LOOP ( 'NONE', ( #5081, #14620, #12983, #191 ) ) ;
#19557 = CARTESIAN_POINT ( 'NONE',  ( -14.48388495494898720, 279.4323905683720568, 9.489475012073731008 ) ) ;
#19558 = CIRCLE ( 'NONE', #20959, 6.500000000000000888 ) ;
#19559 = CARTESIAN_POINT ( 'NONE',  ( -44.16309181155855867, 314.4948905683720000, 6.410867750099241924 ) ) ;
#19560 = CARTESIAN_POINT ( 'NONE',  ( -8.685887942688712116, 266.6823905765655809, 3.978247347593161010 ) ) ;
#19561 = CARTESIAN_POINT ( 'NONE',  ( 160.4540391785681948, 610.7448905601785327, 9.864615503757169890 ) ) ;
#19562 = CARTESIAN_POINT ( 'NONE',  ( -45.43829269268869808, 233.5573905683720568, -3.332260488124726638 ) ) ;
#19563 = CARTESIAN_POINT ( 'NONE',  ( -28.68588794268871567, 372.8698905683720000, -16.75240474999999307 ) ) ;
#19564 = AXIS2_PLACEMENT_3D ( 'NONE', #10514, #10301, #20168 ) ;
#19565 = DIRECTION ( 'NONE',  ( -1.000000000000000000, 0.000000000000000000, 0.000000000000000000 ) ) ;
#19566 = CARTESIAN_POINT ( 'NONE',  ( -10.20829729246297468, 261.6198905601784759, 7.653668647301790529 ) ) ;
#19567 = CARTESIAN_POINT ( 'NONE',  ( -28.68588794268874054, 588.2448905601785327, 0.000000000000000000 ) ) ;
#19568 = VECTOR ( 'NONE', #11045, 1000.000000000000000 ) ;
#19569 = CARTESIAN_POINT ( 'NONE',  ( -45.43829269268871229, 424.1823905683721136, 3.332260488124734632 ) ) ;
#19570 = DIRECTION ( 'NONE',  ( 0.000000000000000000, 0.5000000000000004441, -0.8660254037844383745 ) ) ;
#19571 = VERTEX_POINT ( 'NONE', #9345 ) ;
#19572 = CARTESIAN_POINT ( 'NONE',  ( -24.70764059509555821, 430.0573905601785327, 19.99999999999998934 ) ) ;
#19573 = EDGE_LOOP ( 'NONE', ( #7568, #14493, #9412, #17324 ) ) ;
#19574 = ORIENTED_EDGE ( 'NONE', *, *, #20066, .T. ) ;
#19575 = ORIENTED_EDGE ( 'NONE', *, *, #3372, .F. ) ;
#19576 = CARTESIAN_POINT ( 'NONE',  ( -42.99872675744467188, 207.3681867157733905, -4.490020761129742688 ) ) ;
#19577 = CARTESIAN_POINT ( 'NONE',  ( -40.01497788969913216, 315.6823905601785327, -16.95518130045146421 ) ) ;
#19578 = CARTESIAN_POINT ( 'NONE',  ( 3.458603197740082180, 213.9102039777116602, 33.59072564020503648 ) ) ;
#19579 = EDGE_CURVE ( 'NONE', #7492, #13150, #10860, .T. ) ;
#19580 = CARTESIAN_POINT ( 'NONE',  ( -14.48388495494899608, 349.4323905683720000, 9.489475012073731008 ) ) ;
#19581 = CIRCLE ( 'NONE', #11970, 50.00000000000000000 ) ;
#19582 = CARTESIAN_POINT ( 'NONE',  ( -8.685887942688740537, 506.6823905765656377, 3.978247347593161010 ) ) ;
#19583 = CARTESIAN_POINT ( 'NONE',  ( -11.93348319268872437, 388.5573905683720000, 3.332260488124728415 ) ) ;
#19584 = CARTESIAN_POINT ( 'NONE',  ( 40.42502041961814996, 170.1716627696692683, 20.00000000000000355 ) ) ;
#19585 = CARTESIAN_POINT ( 'NONE',  ( -22.27502019258947996, 386.9948905683720568, 15.47720386886985189 ) ) ;
#19586 = AXIS2_PLACEMENT_3D ( 'NONE', #12150, #18426, #10197 ) ;
#19587 = CARTESIAN_POINT ( 'NONE',  ( -42.82802356641965247, 323.2448905765656377, 14.14213562373094923 ) ) ;
#19588 = DIRECTION ( 'NONE',  ( -1.000000000000000000, 0.000000000000000000, 0.000000000000000000 ) ) ;
#19589 = EDGE_CURVE ( 'NONE', #13633, #5613, #21093, .T. ) ;
#19590 = CARTESIAN_POINT ( 'NONE',  ( -25.35362745456396993, 276.6823905683720000, 16.75240474999998952 ) ) ;
#19591 = CARTESIAN_POINT ( 'NONE',  ( -45.43829269268871229, 445.0573905683720000, -3.332260488124726194 ) ) ;
#19592 = DIRECTION ( 'NONE',  ( 1.191790137725560488E-16, -1.000000000000000000, -0.000000000000000000 ) ) ;
#19593 = DIRECTION ( 'NONE',  ( 0.000000000000000000, 0.000000000000000000, 1.000000000000000000 ) ) ;
#19594 = LINE ( 'NONE', #13336, #3332 ) ;
#19595 = UNCERTAINTY_MEASURE_WITH_UNIT (LENGTH_MEASURE( 1.000000000000000082E-05 ), #4027, 'distance_accuracy_value', 'NONE');
#19596 = DIRECTION ( 'NONE',  ( 1.000000000000000000, 0.000000000000000000, -0.000000000000000000 ) ) ;
#19597 = VECTOR ( 'NONE', #20083, 1000.000000000000000 ) ;
#19598 = CARTESIAN_POINT ( 'NONE',  ( -32.01814843081344719, 357.5573905683720000, 16.75240474999999307 ) ) ;
#19599 = CARTESIAN_POINT ( 'NONE',  ( -35.09675569278796559, 475.7448905683720568, 15.47720386886985366 ) ) ;
#19600 = CARTESIAN_POINT ( 'NONE',  ( -48.68588794268872277, 487.5573905601784759, 3.978247347593168115 ) ) ;
#19601 = CARTESIAN_POINT ( 'NONE',  ( -22.27502019258947286, 326.9948905683720000, 15.47720386886985189 ) ) ;
#19602 = VERTEX_POINT ( 'NONE', #15752 ) ;
#19603 = CARTESIAN_POINT ( 'NONE',  ( -42.82802356641964536, 258.4948905601784759, 14.14213562373094923 ) ) ;
#19604 = PRODUCT ( 'Bronze Screw Shaft Nut Sleeve', 'Bronze Screw Shaft Nut Sleeve', '', ( #11926 ) ) ;
#19605 = ORIENTED_EDGE ( 'NONE', *, *, #11610, .T. ) ;
#19606 = DIRECTION ( 'NONE',  ( 0.000000000000000000, -1.000000000000000000, 0.000000000000000000 ) ) ;
#19607 = EDGE_CURVE ( 'NONE', #19679, #15845, #19092, .T. ) ;
#19608 = CARTESIAN_POINT ( 'NONE',  ( -13.20868407381886378, 409.7448905683720000, 6.410867750099229490 ) ) ;
#19609 = CARTESIAN_POINT ( 'NONE',  ( 20.42502041961813575, 271.1055109169419666, 40.00000000000000000 ) ) ;
#19610 = CARTESIAN_POINT ( 'NONE',  ( -40.53162694259544452, 442.6198905683720568, -11.84573899990672707 ) ) ;
#19611 = CARTESIAN_POINT ( 'NONE',  ( -22.27502019258948707, 446.9948905683720000, 15.47720386886985189 ) ) ;
#19612 = DIRECTION ( 'NONE',  ( 1.000000000000000000, 0.000000000000000000, 0.000000000000000000 ) ) ;
#19613 = FACE_OUTER_BOUND ( 'NONE', #20069, .T. ) ;
#19614 = CARTESIAN_POINT ( 'NONE',  ( -21.03221929538692692, 388.8698905765656377, -18.47759065022572855 ) ) ;
#19615 = CARTESIAN_POINT ( 'NONE',  ( -11.91936617617171734, 51.80349839367686826, 46.68171932492850829 ) ) ;
#19616 = CARTESIAN_POINT ( 'NONE',  ( -28.68588794268870501, 264.7448905601784759, -19.99999999999999289 ) ) ;
#19617 = CARTESIAN_POINT ( 'NONE',  ( -28.68588794268874054, 271.1055109169419666, -40.00000000000000000 ) ) ;
#19618 = CARTESIAN_POINT ( 'NONE',  ( -21.03221929538689849, 255.1198905765656377, 18.47759065022572500 ) ) ;
#19619 = CARTESIAN_POINT ( 'NONE',  ( -25.35362745456399480, 488.1823905683720568, 16.75240474999998952 ) ) ;
#19620 = DIRECTION ( 'NONE',  ( -1.000000000000000000, -0.000000000000000000, -0.000000000000000000 ) ) ;
#19621 = DIRECTION ( 'NONE',  ( -0.000000000000000000, -1.000000000000000000, -0.000000000000000000 ) ) ;
#19622 = LINE ( 'NONE', #68, #17158 ) ;
#19623 = ADVANCED_FACE ( 'NONE', ( #2444 ), #7721, .T. ) ;
#19624 = CARTESIAN_POINT ( 'NONE',  ( -45.43829269268871229, 415.6823905683721136, 3.332260488124734632 ) ) ;
#19625 = CARTESIAN_POINT ( 'NONE',  ( 5.299999999999999822, 7.505553499465139389, 0.000000000000000000 ) ) ;
#19626 = CARTESIAN_POINT ( 'NONE',  ( -45.43829269268869808, 235.3698905683720284, 0.000000000000000000 ) ) ;
#19627 = ORIENTED_EDGE ( 'NONE', *, *, #2237, .T. ) ;
#19628 = CARTESIAN_POINT ( 'NONE',  ( -32.66413529028187668, 424.1823905765656377, 19.99999999999999289 ) ) ;
#19629 = ORIENTED_EDGE ( 'NONE', *, *, #19589, .T. ) ;
#19630 = CARTESIAN_POINT ( 'NONE',  ( -40.53162694259545162, 454.1198905683720568, -11.84573899990672707 ) ) ;
#19631 = CARTESIAN_POINT ( 'NONE',  ( -36.33955658999049376, 230.1198905765656093, -18.47759065022572855 ) ) ;
#19632 = ORIENTED_EDGE ( 'NONE', *, *, #20470, .T. ) ;
#19633 = LINE ( 'NONE', #8052, #7254 ) ;
#19634 = CARTESIAN_POINT ( 'NONE',  ( -19.19641293061500065, 528.8073905683719431, 14.20200298773971426 ) ) ;
#19635 = EDGE_LOOP ( 'NONE', ( #16373, #2778, #8403, #17510, #20304 ) ) ;
#19636 = CARTESIAN_POINT ( 'NONE',  ( -44.16309181155858710, 514.4948905683720568, 6.410867750099241924 ) ) ;
#19637 = LINE ( 'NONE', #16518, #12471 ) ;
#19638 = CARTESIAN_POINT ( 'NONE',  ( -48.68588794268872277, 452.3073905765656377, 3.978247347593168115 ) ) ;
#19639 = CARTESIAN_POINT ( 'NONE',  ( -10.20829729246298534, 357.6198905765656377, -7.653668647301794969 ) ) ;
#19640 = CARTESIAN_POINT ( 'NONE',  ( -21.03221929538690915, 248.8698905765656093, -18.47759065022572855 ) ) ;
#19641 =( NAMED_UNIT ( * ) SI_UNIT ( $, .STERADIAN. ) SOLID_ANGLE_UNIT ( ) );
#19642 = CARTESIAN_POINT ( 'NONE',  ( 91.21585410611801592, 56.85652257517428865, 94.99999999999994316 ) ) ;
#19643 = DIRECTION ( 'NONE',  ( 1.250996701150283068E-16, -1.000000000000000000, 0.000000000000000000 ) ) ;
#19644 = VECTOR ( 'NONE', #5149, 1000.000000000000000 ) ;
#19645 = CARTESIAN_POINT ( 'NONE',  ( 146.1533239063698772, 600.7448905601785327, 7.500000000000000000 ) ) ;
#19646 = CARTESIAN_POINT ( 'NONE',  ( -17.15890915289496732, 223.9102039777116318, -16.43681639555801510 ) ) ;
#19647 = CARTESIAN_POINT ( 'NONE',  ( -11.93348319268871549, 310.3698905683720568, -2.051577885510841163E-15 ) ) ;
#19648 = DIRECTION ( 'NONE',  ( 1.191790137725560488E-16, -1.000000000000000000, 0.000000000000000000 ) ) ;
#19649 = CARTESIAN_POINT ( 'NONE',  ( -28.68588794268869790, 259.7448905601784759, 19.99999999999999289 ) ) ;
#19650 = LINE ( 'NONE', #4830, #10567 ) ;
#19651 = CARTESIAN_POINT ( 'NONE',  ( -38.17536295476244135, 286.9323905683720000, 14.20200298773971781 ) ) ;
#19652 = CARTESIAN_POINT ( 'NONE',  ( -45.43829269268873361, 525.6823905683720568, 3.332260488124734632 ) ) ;
#19653 = CARTESIAN_POINT ( 'NONE',  ( -17.35679799567829207, 370.6823905601784759, 16.95518130045146421 ) ) ;
#19654 = CARTESIAN_POINT ( 'NONE',  ( -48.68588794268853803, 316.9323905601784759, -3.978247347593583783 ) ) ;
#19655 = VERTEX_POINT ( 'NONE', #4276 ) ;
#19656 = CARTESIAN_POINT ( 'NONE',  ( -45.43829269268872650, 495.3698905683720568, 0.000000000000000000 ) ) ;
#19657 = DIRECTION ( 'NONE',  ( -1.191790137725560488E-16, 1.000000000000000000, -0.000000000000000000 ) ) ;
#19658 = CARTESIAN_POINT ( 'NONE',  ( -38.17536295476244135, 285.4323905683720568, 14.20200298773971781 ) ) ;
#19659 = ADVANCED_FACE ( 'NONE', ( #15860 ), #12711, .F. ) ;
#19660 = ORIENTED_EDGE ( 'NONE', *, *, #17782, .T. ) ;
#19661 = EDGE_CURVE ( 'NONE', #3061, #8258, #20508, .T. ) ;
#19662 = CARTESIAN_POINT ( 'NONE',  ( -42.88789093042842637, 276.3073905683720000, 9.489475012073734561 ) ) ;
#19663 = VECTOR ( 'NONE', #13020, 1000.000000000000000 ) ;
#19664 = CARTESIAN_POINT ( 'NONE',  ( -22.27502019258947996, 310.7448905683720000, -15.47720386886985544 ) ) ;
#19665 = CARTESIAN_POINT ( 'NONE',  ( -32.01814843081343298, 257.5573905683720000, 16.75240474999999307 ) ) ;
#19666 = CARTESIAN_POINT ( 'NONE',  ( -24.70764059509554755, 239.1823905765656093, -19.99999999999999289 ) ) ;
#19667 = LINE ( 'NONE', #4961, #5165 ) ;
#19668 = LINE ( 'NONE', #21392, #2008 ) ;
#19669 = CARTESIAN_POINT ( 'NONE',  ( -45.43829269268870519, 375.6823905683720000, 3.332260488124734632 ) ) ;
#19670 = AXIS2_PLACEMENT_3D ( 'NONE', #10691, #15807, #2386 ) ;
#19671 = CARTESIAN_POINT ( 'NONE',  ( -11.73070664223723547, 281.3073905601785327, 11.32908994701042005 ) ) ;
#19672 = CARTESIAN_POINT ( 'NONE',  ( 5.299999999999999822, 7.505553499465139389, 0.000000000000000000 ) ) ;
#19673 =( BOUNDED_CURVE ( )  B_SPLINE_CURVE ( 2, ( #2013, #13581, #178, #18432, #9881, #1909, #3196, #4803, #16504, #11399, #8476, #18001, #6747, #1684, #13144, #9774, #16399 ),
 .UNSPECIFIED., .F., .T. ) 
 B_SPLINE_CURVE_WITH_KNOTS ( ( 3, 2, 2, 2, 2, 2, 2, 2, 3 ),
 ( 0.1875000000000001665, 0.1894531250000001665, 0.1914062500000001665, 0.1933593750000001665, 0.1953125000000001665, 0.1972656250000001665, 0.1992187500000001665, 0.2011718750000001665, 0.2031250000000001665 ),
 .UNSPECIFIED. ) 
 CURVE ( )  GEOMETRIC_REPRESENTATION_ITEM ( )  RATIONAL_B_SPLINE_CURVE ( ( 0.9999999999999983347, 0.9807852804032320959, 1.000000000000000000, 0.9807852804032304306, 1.000000000000000000, 0.9807852804032304306, 1.000000000000000000, 0.9807852804032304306, 1.000000000000000000, 0.9807852804032304306, 1.000000000000000000, 0.9807852804032304306, 1.000000000000000000, 0.9807852804032304306, 1.000000000000000000, 0.9807852804032287652, 1.000000000000001554 ) ) 
 REPRESENTATION_ITEM ( '' )  );
#19674 = CARTESIAN_POINT ( 'NONE',  ( -8.685887942688534480, 267.3073905765655240, -3.978247347592740013 ) ) ;
#19675 = CARTESIAN_POINT ( 'NONE',  ( -19.19641293061498999, 430.4323905683720000, -14.20200298773971603 ) ) ;
#19676 = DIRECTION ( 'NONE',  ( 1.000000000000000000, 0.000000000000000000, 0.000000000000000000 ) ) ;
#19677 = VERTEX_POINT ( 'NONE', #14767 ) ;
#19678 = CARTESIAN_POINT ( 'NONE',  ( -28.68588794268871922, 429.7448905601785327, 19.99999999999999289 ) ) ;
#19679 = VERTEX_POINT ( 'NONE', #17884 ) ;
#19680 = FACE_OUTER_BOUND ( 'NONE', #743, .T. ) ;
#19681 = ORIENTED_EDGE ( 'NONE', *, *, #13058, .F. ) ;
#19682 = VERTEX_POINT ( 'NONE', #19945 ) ;
#19683 = DIRECTION ( 'NONE',  ( 0.000000000000000000, 0.000000000000000000, -1.000000000000000000 ) ) ;
#19684 = CARTESIAN_POINT ( 'NONE',  ( -48.68588794268870146, 297.2448905601784759, 0.000000000000000000 ) ) ;
#19685 = DIRECTION ( 'NONE',  ( 1.191790137725560488E-16, -1.000000000000000000, 0.000000000000000000 ) ) ;
#19686 = CARTESIAN_POINT ( 'NONE',  ( -28.68588794268871212, 347.8698905683720568, 16.75240474999999307 ) ) ;
#19687 = CARTESIAN_POINT ( 'NONE',  ( -24.70764059509556532, 484.8073905765656946, 19.99999999999998934 ) ) ;
#19688 = CARTESIAN_POINT ( 'NONE',  ( -45.43829269268871229, 373.8698905683720000, 0.000000000000000000 ) ) ;
#19689 = PLANE ( 'NONE',  #5135 ) ;
#19690 = CARTESIAN_POINT ( 'NONE',  ( -28.68588794268871922, 381.3698905683720568, -16.75240474999999307 ) ) ;
#19691 = CARTESIAN_POINT ( 'NONE',  ( -40.01497788969912506, 323.5573905765655809, 16.95518130045146776 ) ) ;
#19692 = CARTESIAN_POINT ( 'NONE',  ( -28.68588794268872277, 424.7448905601784759, -19.99999999999999289 ) ) ;
#19693 = CARTESIAN_POINT ( 'NONE',  ( -16.84014894278198327, 290.1198905683720568, -11.84573899990672707 ) ) ;
#19694 = CARTESIAN_POINT ( 'NONE',  ( -14.54375231895777532, 440.9948905601784759, 14.14213562373094568 ) ) ;
#19695 = CARTESIAN_POINT ( 'NONE',  ( -42.88789093042844058, 446.3073905683720000, 9.489475012073736337 ) ) ;
#19696 = FACE_OUTER_BOUND ( 'NONE', #18672, .T. ) ;
#19697 = CARTESIAN_POINT ( 'NONE',  ( 0.05613245601076820995, 1.278525034532179250, 6.500000000000002665 ) ) ;
#19698 = DIRECTION ( 'NONE',  ( 0.000000000000000000, 0.000000000000000000, 1.000000000000000000 ) ) ;
#19699 = DIRECTION ( 'NONE',  ( -1.191790137725560488E-16, 1.000000000000000000, -0.000000000000000000 ) ) ;
#19700 = AXIS2_PLACEMENT_3D ( 'NONE', #15093, #171, #6846 ) ;
#19701 = CARTESIAN_POINT ( 'NONE',  ( -42.88789093042843348, 354.4323905683720568, -9.489475012073736337 ) ) ;
#19702 = CARTESIAN_POINT ( 'NONE',  ( -28.68588794268873343, 491.3698905683720568, -16.75240474999999307 ) ) ;
#19703 = VERTEX_POINT ( 'NONE', #3077 ) ;
#19704 = CARTESIAN_POINT ( 'NONE',  ( -17.35679799567830628, 490.6823905601784759, 16.95518130045146421 ) ) ;
#19705 = CARTESIAN_POINT ( 'NONE',  ( -14.48388495494899075, 307.9323905683720000, 9.489475012073732785 ) ) ;
#19706 = ORIENTED_EDGE ( 'NONE', *, *, #21068, .T. ) ;
#19707 = AXIS2_PLACEMENT_3D ( 'NONE', #9232, #5770, #10743 ) ;
#19708 = CIRCLE ( 'NONE', #4853, 28.29169339157297358 ) ;
#19709 = CARTESIAN_POINT ( 'NONE',  ( -28.68588794268869790, 259.7448905601784759, 19.99999999999999289 ) ) ;
#19710 = ORIENTED_EDGE ( 'NONE', *, *, #7363, .T. ) ;
#19711 = CARTESIAN_POINT ( 'NONE',  ( -28.68588794268873343, 47.23886018424757083, 49.60091809715359545 ) ) ;
#19712 = ADVANCED_FACE ( 'NONE', ( #2978 ), #16602, .T. ) ;
#19713 = AXIS2_PLACEMENT_3D ( 'NONE', #14816, #14421, #4449 ) ;
#19714 = CARTESIAN_POINT ( 'NONE',  ( -38.17536295476246266, 403.8073905683721136, -14.20200298773971426 ) ) ;
#19715 = CYLINDRICAL_SURFACE ( 'NONE', #14208, 19.99999999999999645 ) ;
#19716 = DIRECTION ( 'NONE',  ( -1.191790137725560488E-16, 1.000000000000000000, -0.000000000000000000 ) ) ;
#19717 = CARTESIAN_POINT ( 'NONE',  ( -42.88789093042844058, 444.8073905683720568, 9.489475012073736337 ) ) ;
#19718 = CARTESIAN_POINT ( 'NONE',  ( -28.68588794268872633, 451.3698905683720000, -16.75240474999999307 ) ) ;
#19719 = CARTESIAN_POINT ( 'NONE',  ( 0.000000000000000000, 0.000000000000000000, 0.000000000000000000 ) ) ;
#19720 = DIRECTION ( 'NONE',  ( 0.000000000000000000, 1.000000000000000000, 0.000000000000000000 ) ) ;
#19721 = LINE ( 'NONE', #20384, #16368 ) ;
#19722 = CARTESIAN_POINT ( 'NONE',  ( -14.54375231895777354, 388.2448905765655809, -14.14213562373094746 ) ) ;
#19723 = CARTESIAN_POINT ( 'NONE',  ( -24.85377105065298764, 45.59741950151473588, 49.45332593944714716 ) ) ;
#19724 = DIRECTION ( 'NONE',  ( 0.000000000000000000, 1.000000000000000000, 9.855701800883825964E-17 ) ) ;
#19725 = CARTESIAN_POINT ( 'NONE',  ( -40.01497788969914637, 430.4323905765655809, -16.95518130045146421 ) ) ;
#19726 = LINE ( 'NONE', #16603, #18317 ) ;
#19727 = CARTESIAN_POINT ( 'NONE',  ( -42.88789093042845479, 506.3073905683720568, 9.489475012073736337 ) ) ;
#19728 = CIRCLE ( 'NONE', #20412, 15.00000000000000000 ) ;
#19729 = CYLINDRICAL_SURFACE ( 'NONE', #12680, 19.99999999999999645 ) ;
#19730 = CARTESIAN_POINT ( 'NONE',  ( -17.35679799567830628, 463.8073905601784190, -16.95518130045146421 ) ) ;
#19731 = CARTESIAN_POINT ( 'NONE',  ( -42.82802356641968089, 518.4948905601785327, 14.14213562373094923 ) ) ;
#19732 = ADVANCED_FACE ( 'NONE', ( #6411 ), #4794, .T. ) ;
#19733 = CARTESIAN_POINT ( 'NONE',  ( -11.93348319268872615, 410.0573905683720000, 3.332260488124728415 ) ) ;
#19734 = LINE ( 'NONE', #393, #12329 ) ;
#19735 = CARTESIAN_POINT ( 'NONE',  ( -40.53162694259542320, 236.6198905683720284, 11.84573899990672885 ) ) ;
#19736 = ORIENTED_EDGE ( 'NONE', *, *, #2411, .T. ) ;
#19737 = DIRECTION ( 'NONE',  ( 0.000000000000000000, -0.000000000000000000, 1.000000000000000000 ) ) ;
#19738 = ORIENTED_EDGE ( 'NONE', *, *, #11264, .F. ) ;
#19739 = CARTESIAN_POINT ( 'NONE',  ( -25.35362745456400191, 452.5573905683720568, -16.75240474999999307 ) ) ;
#19740 = CARTESIAN_POINT ( 'NONE',  ( -14.54375231895775045, 225.7448905765656093, 14.14213562373094568 ) ) ;
#19741 = ORIENTED_EDGE ( 'NONE', *, *, #4546, .T. ) ;
#19742 = CONICAL_SURFACE ( 'NONE', #771, 6.500000000000000000, 1.047197551196600296 ) ;
#19743 = CARTESIAN_POINT ( 'NONE',  ( -48.68588794268875120, 522.3073905765655809, 3.978247347593114824 ) ) ;
#19744 = CARTESIAN_POINT ( 'NONE',  ( -21.25395633610896695, 220.6412455016266279, -15.05426537146665389 ) ) ;
#19745 = ORIENTED_EDGE ( 'NONE', *, *, #19396, .T. ) ;
#19746 = CARTESIAN_POINT ( 'NONE',  ( -32.01814843081345430, 501.6823905683720568, -16.75240474999999307 ) ) ;
#19747 = CARTESIAN_POINT ( 'NONE',  ( 0.4033376246892498296, 7.198601258566900363, -0.5316568767328675449 ) ) ;
#19748 = EDGE_CURVE ( 'NONE', #15635, #15821, #16532, .T. ) ;
#19749 = CARTESIAN_POINT ( 'NONE',  ( -48.68588794268871567, 442.3073905765656377, 3.978247347593168115 ) ) ;
#19750 = DIRECTION ( 'NONE',  ( -0.000000000000000000, -0.000000000000000000, -1.000000000000000000 ) ) ;
#19751 = CARTESIAN_POINT ( 'NONE',  ( -36.33955658999050797, 329.1198905601784759, 18.47759065022572500 ) ) ;
#19752 = PLANE ( 'NONE',  #9436 ) ;
#19753 = LINE ( 'NONE', #1175, #8712 ) ;
#19754 = CARTESIAN_POINT ( 'NONE',  ( 158.8141120573112630, 400.5398297725603243, 9.999999999999980460 ) ) ;
#19755 =( NAMED_UNIT ( * ) SI_UNIT ( $, .STERADIAN. ) SOLID_ANGLE_UNIT ( ) );
#19756 = CARTESIAN_POINT ( 'NONE',  ( -8.685887942688738761, 496.9948905765655809, -2.449293598294705724E-15 ) ) ;
#19757 = CARTESIAN_POINT ( 'NONE',  ( -13.20868407381885312, 319.7448905683720000, 6.410867750099229490 ) ) ;
#19758 = ADVANCED_FACE ( 'NONE', ( #8034 ), #13136, .F. ) ;
#19759 = CARTESIAN_POINT ( 'NONE',  ( -48.68588794268860198, 236.9323905601785043, -3.978247347593371508 ) ) ;
#19760 = CARTESIAN_POINT ( 'NONE',  ( -28.68588794268870501, 274.7448905601784759, -19.99999999999999289 ) ) ;
#19761 = DIRECTION ( 'NONE',  ( -1.191790137725560488E-16, 1.000000000000000000, -0.000000000000000000 ) ) ;
#19762 = CARTESIAN_POINT ( 'NONE',  ( -45.43829269268869808, 285.6823905683720000, 3.332260488124734632 ) ) ;
#19763 = CARTESIAN_POINT ( 'NONE',  ( -35.09675569278795848, 503.4948905683720568, -15.47720386886985544 ) ) ;
#19764 = CARTESIAN_POINT ( 'NONE',  ( -24.70764059509555111, 370.0573905601783622, 19.99999999999998934 ) ) ;
#19765 = ORIENTED_EDGE ( 'NONE', *, *, #21337, .T. ) ;
#19766 = CARTESIAN_POINT ( 'NONE',  ( -16.84014894278200103, 479.1198905683720000, 11.84573899990672530 ) ) ;
#19767 = FILL_AREA_STYLE ('',( #3018 ) ) ;
#19768 = CARTESIAN_POINT ( 'NONE',  ( -40.53162694259543031, 275.1198905683720568, 11.84573899990672885 ) ) ;
#19769 = VECTOR ( 'NONE', #17157, 1000.000000000000000 ) ;
#19770 = ORIENTED_EDGE ( 'NONE', *, *, #4862, .T. ) ;
#19771 = FACE_OUTER_BOUND ( 'NONE', #20841, .T. ) ;
#19772 = CARTESIAN_POINT ( 'NONE',  ( -35.09675569278794427, 287.2448905683720000, 15.47720386886985366 ) ) ;
#19773 = CARTESIAN_POINT ( 'NONE',  ( -42.88789093042841927, 254.4323905683720284, -9.489475012073734561 ) ) ;
#19774 = CARTESIAN_POINT ( 'NONE',  ( -48.68588794268869435, 251.9948905765656093, 0.000000000000000000 ) ) ;
#19775 = CARTESIAN_POINT ( 'NONE',  ( -8.685887942688742314, 573.2448905601785327, 2.449293598294706119E-15 ) ) ;
#19776 = LINE ( 'NONE', #19352, #16852 ) ;
#19777 = CARTESIAN_POINT ( 'NONE',  ( -42.88789093042841927, 264.8073905683721136, 9.489475012073736337 ) ) ;
#19778 = CARTESIAN_POINT ( 'NONE',  ( -11.93348319268872260, 380.0573905683721136, 3.332260488124728415 ) ) ;
#19779 = FACE_OUTER_BOUND ( 'NONE', #6431, .T. ) ;
#19780 = CARTESIAN_POINT ( 'NONE',  ( -10.20829729246299777, 457.6198905765656377, -7.653668647301794969 ) ) ;
#19781 = PRODUCT_DEFINITION_SHAPE ( 'NONE', 'NONE',  #21396 ) ;
#19782 = EDGE_CURVE ( 'NONE', #19453, #9142, #3187, .T. ) ;
#19783 = AXIS2_PLACEMENT_3D ( 'NONE', #5626, #16897, #18711 ) ;
#19784 = CARTESIAN_POINT ( 'NONE',  ( 162.8695233526006803, 610.7448905601785327, -10.81142786866620575 ) ) ;
#19785 = ADVANCED_FACE ( 'NONE', ( #6519 ), #1566, .F. ) ;
#19786 = CARTESIAN_POINT ( 'NONE',  ( -44.16309181155857999, 413.2448905683720568, -6.410867750099231266 ) ) ;
#19787 = CARTESIAN_POINT ( 'NONE',  ( 30.42502041961813575, 271.1055109169419097, -40.00000000000000000 ) ) ;
#19788 = ORIENTED_EDGE ( 'NONE', *, *, #5960, .F. ) ;
#19789 = CARTESIAN_POINT ( 'NONE',  ( -45.64106924314019409, 428.1823905601784759, 11.32908994701042715 ) ) ;
#19790 = ORIENTED_EDGE ( 'NONE', *, *, #9878, .F. ) ;
#19791 = ORIENTED_EDGE ( 'NONE', *, *, #18214, .F. ) ;
#19792 = ORIENTED_EDGE ( 'NONE', *, *, #4453, .T. ) ;
#19793 = CARTESIAN_POINT ( 'NONE',  ( -48.68588794268880093, 352.3073905765656377, 3.978247347592954952 ) ) ;
#19794 = CARTESIAN_POINT ( 'NONE',  ( -42.82802356641965247, 305.9948905601784759, -14.14213562373094746 ) ) ;
#19795 = LINE ( 'NONE', #16564, #16644 ) ;
#19796 = ADVANCED_FACE ( 'NONE', ( #8248 ), #1792, .F. ) ;
#19797 = CIRCLE ( 'NONE', #12554, 5.000000000000001776 ) ;
#19798 = CARTESIAN_POINT ( 'NONE',  ( -38.17536295476245556, 353.8073905683720568, -14.20200298773971426 ) ) ;
#19799 = ORIENTED_EDGE ( 'NONE', *, *, #11993, .F. ) ;
#19800 = CARTESIAN_POINT ( 'NONE',  ( -14.54375231895778597, 488.2448905765656377, -14.14213562373094746 ) ) ;
#19801 = CARTESIAN_POINT ( 'NONE',  ( -32.01814843081344719, 361.6823905683720568, -16.75240474999999307 ) ) ;
#19802 = DIRECTION ( 'NONE',  ( 0.000000000000000000, 0.000000000000000000, 1.000000000000000000 ) ) ;
#19803 = EDGE_CURVE ( 'NONE', #2116, #6373, #19461, .T. ) ;
#19804 = AXIS2_PLACEMENT_3D ( 'NONE', #5040, #8387, #18344 ) ;
#19805 = CARTESIAN_POINT ( 'NONE',  ( -40.53162694259543741, 382.6198905683720568, -11.84573899990672707 ) ) ;
#19806 = EDGE_CURVE ( 'NONE', #5497, #451, #836, .T. ) ;
#19807 = CARTESIAN_POINT ( 'NONE',  ( -11.73070664223723902, 306.0573905765655809, 11.32908994701042005 ) ) ;
#19808 = DIRECTION ( 'NONE',  ( 0.000000000000000000, 0.000000000000000000, 1.000000000000000000 ) ) ;
#19809 = CARTESIAN_POINT ( 'NONE',  ( -44.16309181155855867, 294.4948905683720000, 6.410867750099241924 ) ) ;
#19810 = DIRECTION ( 'NONE',  ( -1.000000000000000000, 0.000000000000000000, 0.000000000000000000 ) ) ;
#19811 =( BOUNDED_CURVE ( )  B_SPLINE_CURVE ( 2, ( #6366, #12975, #19566, #12695, #16058, #19392, #21233, #19500, #19709, #19287, #1551, #12910, #19603, #1337, #4577, #4679, #2857 ),
 .UNSPECIFIED., .F., .T. ) 
 B_SPLINE_CURVE_WITH_KNOTS ( ( 3, 2, 2, 2, 2, 2, 2, 2, 3 ),
 ( 0.8593750000000002220, 0.8613281250000002220, 0.8632812500000002220, 0.8652343750000002220, 0.8671875000000002220, 0.8691406250000002220, 0.8710937500000002220, 0.8730468750000002220, 0.8750000000000002220 ),
 .UNSPECIFIED. ) 
 CURVE ( )  GEOMETRIC_REPRESENTATION_ITEM ( )  RATIONAL_B_SPLINE_CURVE ( ( 0.9999999999999977796, 0.9807852804032326510, 1.000000000000000000, 0.9807852804032304306, 1.000000000000000000, 0.9807852804032304306, 1.000000000000000000, 0.9807852804032304306, 1.000000000000000000, 0.9807852804032304306, 1.000000000000000000, 0.9807852804032304306, 1.000000000000000000, 0.9807852804032304306, 1.000000000000000000, 0.9807852804032282101, 1.000000000000002220 ) ) 
 REPRESENTATION_ITEM ( '' )  );
#19812 = CARTESIAN_POINT ( 'NONE',  ( -28.68588794268872277, 437.8698905683720568, 16.75240474999999307 ) ) ;
#19813 = CYLINDRICAL_SURFACE ( 'NONE', #18554, 20.00000000000000000 ) ;
#19814 = CARTESIAN_POINT ( 'NONE',  ( -14.54375231895778775, 513.4948905601785327, -14.14213562373094746 ) ) ;
#19815 = CARTESIAN_POINT ( 'NONE',  ( 0.5805565836007597902, 3.752776749732560368, -6.499999999999999112 ) ) ;
#19816 = LINE ( 'NONE', #18293, #16469 ) ;
#19817 = EDGE_CURVE ( 'NONE', #17482, #12966, #18101, .T. ) ;
#19818 = VECTOR ( 'NONE', #14254, 1000.000000000000000 ) ;
#19819 = CARTESIAN_POINT ( 'NONE',  ( -11.93348319268872260, 350.0573905683720000, 3.332260488124728415 ) ) ;
#19820 = CARTESIAN_POINT ( 'NONE',  ( -28.68588794268872633, 476.3698905683720568, 16.75240474999999307 ) ) ;
#19821 = AXIS2_PLACEMENT_3D ( 'NONE', #21194, #12441, #12871 ) ;
#19822 = ORIENTED_EDGE ( 'NONE', *, *, #3803, .F. ) ;
#19823 = CARTESIAN_POINT ( 'NONE',  ( -21.03221929538693757, 484.1198905601785327, -18.47759065022572855 ) ) ;
#19824 = CARTESIAN_POINT ( 'NONE',  ( -45.43829269268870519, 293.8698905683720568, 0.000000000000000000 ) ) ;
#19825 = AXIS2_PLACEMENT_3D ( 'NONE', #3140, #14509, #9722 ) ;
#19826 = ORIENTED_EDGE ( 'NONE', *, *, #14057, .T. ) ;
#19827 = VERTEX_POINT ( 'NONE', #19838 ) ;
#19828 = LINE ( 'NONE', #3285, #11200 ) ;
#19829 = CARTESIAN_POINT ( 'NONE',  ( -45.43829269268871940, 395.6823905683719431, 3.332260488124734632 ) ) ;
#19830 = DIRECTION ( 'NONE',  ( -1.000000000000000000, 0.000000000000000000, 0.000000000000000000 ) ) ;
#19831 = DIRECTION ( 'NONE',  ( -1.000000000000000000, 0.000000000000000000, 0.000000000000000000 ) ) ;
#19832 = CARTESIAN_POINT ( 'NONE',  ( -45.43829269268871229, 434.1823905683720568, 3.332260488124734632 ) ) ;
#19833 = CARTESIAN_POINT ( 'NONE',  ( -38.17536295476245556, 445.4323905683720000, 14.20200298773971781 ) ) ;
#19834 = CARTESIAN_POINT ( 'NONE',  ( -48.68588794268873698, 573.2448905601785327, 0.000000000000000000 ) ) ;
#19835 = CARTESIAN_POINT ( 'NONE',  ( -10.20829729246298712, 367.6198905765656377, -7.653668647301794969 ) ) ;
#19836 = CARTESIAN_POINT ( 'NONE',  ( -10.80396482869975472, 55.79733835392248409, 46.26547175773355747 ) ) ;
#19837 = DIRECTION ( 'NONE',  ( 1.000000000000000000, 0.000000000000000000, 0.000000000000000000 ) ) ;
#19838 = CARTESIAN_POINT ( 'NONE',  ( 60.69669829156632090, 56.85652257517428865, 94.99999999999994316 ) ) ;
#19839 = CARTESIAN_POINT ( 'NONE',  ( 0.000000000000000000, 7.960204194457796463E-16, -6.500000000000000888 ) ) ;
#19840 = VECTOR ( 'NONE', #17976, 1000.000000000000000 ) ;
#19841 = CARTESIAN_POINT ( 'NONE',  ( -38.17536295476246977, 506.9323905683720568, 14.20200298773971781 ) ) ;
#19842 = DIRECTION ( 'NONE',  ( 0.000000000000000000, 0.000000000000000000, -1.000000000000000000 ) ) ;
#19843 = DIRECTION ( 'NONE',  ( 0.000000000000000000, 0.000000000000000000, -1.000000000000000000 ) ) ;
#19844 = CARTESIAN_POINT ( 'NONE',  ( -14.48388495494900496, 399.4323905683720568, 9.489475012073732785 ) ) ;
#19845 = LINE ( 'NONE', #8256, #18530 ) ;
#19846 = CARTESIAN_POINT ( 'NONE',  ( -44.16309181155855157, 235.9948905683720284, 6.410867750099241924 ) ) ;
#19847 = CARTESIAN_POINT ( 'NONE',  ( -38.17536295476245556, 372.3073905683721136, -14.20200298773971426 ) ) ;
#19848 = ORIENTED_EDGE ( 'NONE', *, *, #16181, .T. ) ;
#19849 = CARTESIAN_POINT ( 'NONE',  ( -42.88789093042845479, 532.9323905683720568, -9.489475012073736337 ) ) ;
#19850 = VERTEX_POINT ( 'NONE', #5014 ) ;
#19851 = CARTESIAN_POINT ( 'NONE',  ( -13.20868407381887089, 450.9948905683720000, -6.410867750099233042 ) ) ;
#19852 = CARTESIAN_POINT ( 'NONE',  ( -14.48388495494901740, 517.9323905683720568, 9.489475012073732785 ) ) ;
#19853 = VERTEX_POINT ( 'NONE', #11614 ) ;
#19854 = CARTESIAN_POINT ( 'NONE',  ( -28.68588794268871922, 429.7448905601785327, 19.99999999999999289 ) ) ;
#19855 = CARTESIAN_POINT ( 'NONE',  ( -35.09675569278796559, 485.7448905683720568, 15.47720386886985366 ) ) ;
#19856 = EDGE_LOOP ( 'NONE', ( #19826, #1193, #3630 ) ) ;
#19857 = CARTESIAN_POINT ( 'NONE',  ( -13.20868407381887621, 498.2448905683720000, 6.410867750099229490 ) ) ;
#19858 = CARTESIAN_POINT ( 'NONE',  ( -15.10870380797810952, 47.82216028940542429, -47.70846432324336917 ) ) ;
#19859 = ADVANCED_FACE ( 'NONE', ( #18205 ), #6740, .F. ) ;
#19860 = CARTESIAN_POINT ( 'NONE',  ( -47.16347859291445843, 452.6198905765656377, 7.653668647301805628 ) ) ;
#19861 = CARTESIAN_POINT ( 'NONE',  ( -42.82802356641965247, 300.7448905765656377, -14.14213562373094746 ) ) ;
#19862 = CARTESIAN_POINT ( 'NONE',  ( -28.68588794268870146, 249.4948905765656093, -19.99999999999999289 ) ) ;
#19863 = DIRECTION ( 'NONE',  ( -1.000000000000000000, 0.000000000000000000, 0.000000000000000000 ) ) ;
#19864 = FACE_OUTER_BOUND ( 'NONE', #14044, .T. ) ;
#19865 = LINE ( 'NONE', #11642, #6346 ) ;
#19866 = CARTESIAN_POINT ( 'NONE',  ( -48.68588794268871567, 437.2448905601785327, 0.000000000000000000 ) ) ;
#19867 = PRODUCT_DEFINITION ( 'UNKNOWN', '', #17655, #11802 ) ;
#19868 = DIRECTION ( 'NONE',  ( 1.374938938973709817E-16, -1.000000000000000000, 0.000000000000000000 ) ) ;
#19869 = CARTESIAN_POINT ( 'NONE',  ( -42.88789093042842637, 306.3073905683719431, 9.489475012073736337 ) ) ;
#19870 = CARTESIAN_POINT ( 'NONE',  ( -40.01497788969915348, 528.8073905601785327, 16.95518130045146776 ) ) ;
#19871 = CARTESIAN_POINT ( 'NONE',  ( -21.03221929538691271, 274.1198905601784759, -18.47759065022572855 ) ) ;
#19872 = CARTESIAN_POINT ( 'NONE',  ( -24.70764059509555466, 414.8073905765656946, 19.99999999999998934 ) ) ;
#19873 = CARTESIAN_POINT ( 'NONE',  ( -11.93348319268871371, 290.6823905683721136, -3.332260488124732856 ) ) ;
#19874 = ADVANCED_FACE ( 'NONE', ( #19913 ), #8110, .T. ) ;
#19875 = CARTESIAN_POINT ( 'NONE',  ( -28.68588794268872988, 507.8698905683720568, 16.75240474999999307 ) ) ;
#19876 = DIRECTION ( 'NONE',  ( -0.000000000000000000, -1.000000000000000000, -0.000000000000000000 ) ) ;
#19877 = VERTEX_POINT ( 'NONE', #6714 ) ;
#19878 = CARTESIAN_POINT ( 'NONE',  ( -38.17536295476246977, 463.8073905683720000, -14.20200298773971426 ) ) ;
#19879 = LINE ( 'NONE', #10340, #21139 ) ;
#19880 = CARTESIAN_POINT ( 'NONE',  ( -28.68588794268870501, 271.3698905683720000, -16.75240474999999307 ) ) ;
#19881 = ORIENTED_EDGE ( 'NONE', *, *, #18880, .F. ) ;
#19882 = CARTESIAN_POINT ( 'NONE',  ( 0.01372220897662236594, -5.948365447239591042, -2.697128823393882158 ) ) ;
#19883 = ADVANCED_FACE ( 'NONE', ( #5094 ), #1539, .T. ) ;
#19884 = CARTESIAN_POINT ( 'NONE',  ( -22.27502019258947641, 272.2448905683720568, -15.47720386886985544 ) ) ;
#19885 = CARTESIAN_POINT ( 'NONE',  ( -35.09675569278793716, 257.2448905683720000, 15.47720386886985366 ) ) ;
#19886 = CARTESIAN_POINT ( 'NONE',  ( -24.70764059509554755, 249.1823905765656093, -19.99999999999999289 ) ) ;
#19887 = FACE_OUTER_BOUND ( 'NONE', #14568, .T. ) ;
#19888 = CARTESIAN_POINT ( 'NONE',  ( -10.20829729246297113, 232.8698905601784759, -7.653668647301794969 ) ) ;
#19889 = CARTESIAN_POINT ( 'NONE',  ( 91.21585410611801592, 31.85652257517428865, -40.00000000000000000 ) ) ;
#19890 = CARTESIAN_POINT ( 'NONE',  ( -28.68588794268870146, 276.3698905683720000, 16.75240474999999307 ) ) ;
#19891 = CARTESIAN_POINT ( 'NONE',  ( -38.17536295476245556, 363.8073905683720568, -14.20200298773971426 ) ) ;
#19892 = CARTESIAN_POINT ( 'NONE',  ( -21.03221929538690205, 280.3698905601784759, 18.47759065022572500 ) ) ;
#19893 = DIRECTION ( 'NONE',  ( 0.000000000000000000, 1.000000000000000000, -0.000000000000000000 ) ) ;
#19894 = CARTESIAN_POINT ( 'NONE',  ( -25.35362745456398770, 426.6823905683720568, 16.75240474999998952 ) ) ;
#19895 = LINE ( 'NONE', #18375, #154 ) ;
#19896 = ORIENTED_EDGE ( 'NONE', *, *, #18409, .F. ) ;
#19897 = CARTESIAN_POINT ( 'NONE',  ( -8.685887942688729879, 432.5573905601785327, -3.978247347593165895 ) ) ;
#19898 = ORIENTED_EDGE ( 'NONE', *, *, #17107, .F. ) ;
#19899 = ORIENTED_EDGE ( 'NONE', *, *, #16104, .T. ) ;
#19900 = ORIENTED_EDGE ( 'NONE', *, *, #1284, .T. ) ;
#19901 = CARTESIAN_POINT ( 'NONE',  ( -35.09675569278796559, 523.4948905683720568, -15.47720386886985544 ) ) ;
#19902 = CARTESIAN_POINT ( 'NONE',  ( -17.35679799567828496, 310.6823905601784759, 16.95518130045146421 ) ) ;
#19903 = CARTESIAN_POINT ( 'NONE',  ( 292.4526463419396691, 308.2087638784415162, 40.00000000000000000 ) ) ;
#19904 = CARTESIAN_POINT ( 'NONE',  ( -35.09675569278795138, 347.2448905683720000, 15.47720386886985366 ) ) ;
#19905 = ORIENTED_EDGE ( 'NONE', *, *, #13998, .T. ) ;
#19906 = CARTESIAN_POINT ( 'NONE',  ( -32.66413529028189089, 479.8073905765655809, -19.99999999999999289 ) ) ;
#19907 = CARTESIAN_POINT ( 'NONE',  ( -16.84014894278199037, 360.1198905683720000, -11.84573899990672707 ) ) ;
#19908 = CARTESIAN_POINT ( 'NONE',  ( -45.43829269268871229, 363.8698905683720000, 0.000000000000000000 ) ) ;
#19909 = AXIS2_PLACEMENT_3D ( 'NONE', #5974, #12585, #6288 ) ;
#19910 = CARTESIAN_POINT ( 'NONE',  ( -42.82802356641965247, 300.7448905765656377, -14.14213562373094746 ) ) ;
#19911 = DIRECTION ( 'NONE',  ( 1.000000000000000000, 0.000000000000000000, 0.000000000000000000 ) ) ;
#19912 = CARTESIAN_POINT ( 'NONE',  ( -25.35362745456398059, 271.0573905683719431, -16.75240474999999307 ) ) ;
#19913 = FACE_OUTER_BOUND ( 'NONE', #16510, .T. ) ;
#19914 = CARTESIAN_POINT ( 'NONE',  ( -22.27502019258949773, 442.2448905683720000, -15.47720386886985544 ) ) ;
#19915 = AXIS2_PLACEMENT_3D ( 'NONE', #647, #9162, #14164 ) ;
#19916 = CARTESIAN_POINT ( 'NONE',  ( 5.674999999999999822, 7.505553499465139389, 0.000000000000000000 ) ) ;
#19917 = CARTESIAN_POINT ( 'NONE',  ( 91.21585410611801592, 56.85652257517428865, 94.99999999999994316 ) ) ;
#19918 = CARTESIAN_POINT ( 'NONE',  ( 0.05613245601036562227, 1.278525034529254034, -6.499999999999999112 ) ) ;
#19919 = CARTESIAN_POINT ( 'NONE',  ( -28.68588794268874054, 573.2448905601785327, 0.000000000000000000 ) ) ;
#19920 = B_SPLINE_CURVE_WITH_KNOTS ( 'NONE', 3,
 ( #13094, #6802, #8531, #8635, #340, #9829 ),
 .UNSPECIFIED., .F., .F.,
 ( 4, 2, 4 ),
 ( 0.01913986446825127058, 0.02104055318008570680, 0.02294124189192014301 ),
 .UNSPECIFIED. ) ;
#19921 = ADVANCED_FACE ( 'NONE', ( #18178 ), #11475, .F. ) ;
#19922 = CARTESIAN_POINT ( 'NONE',  ( -45.43829269268870519, 355.0573905683720568, -3.332260488124726194 ) ) ;
#19923 = CARTESIAN_POINT ( 'NONE',  ( -42.88789093042844769, 482.9323905683720568, -9.489475012073736337 ) ) ;
#19924 = ADVANCED_FACE ( 'NONE', ( #11586 ), #16467, .T. ) ;
#19925 = ORIENTED_EDGE ( 'NONE', *, *, #16291, .F. ) ;
#19926 = CARTESIAN_POINT ( 'NONE',  ( -32.66413529028189089, 485.0573905601785327, -19.99999999999999289 ) ) ;
#19927 = CARTESIAN_POINT ( 'NONE',  ( -32.01814843081344009, 301.6823905683720568, -16.75240474999999307 ) ) ;
#19928 = EDGE_CURVE ( 'NONE', #18459, #15711, #11870, .T. ) ;
#19929 = AXIS2_PLACEMENT_3D ( 'NONE', #10625, #498, #10516 ) ;
#19930 = CARTESIAN_POINT ( 'NONE',  ( -41.83569717483972994, 230.5765313837437418, 25.00000000000000000 ) ) ;
#19931 = EDGE_LOOP ( 'NONE', ( #9969, #13640, #2061, #4534, #8408 ) ) ;
#19932 = DIRECTION ( 'NONE',  ( 0.000000000000000000, -0.000000000000000000, -1.000000000000000000 ) ) ;
#19933 = CARTESIAN_POINT ( 'NONE',  ( -19.19641293061498999, 411.9323905683720000, -14.20200298773971603 ) ) ;
#19934 = CARTESIAN_POINT ( 'NONE',  ( -48.68588794268872277, 477.2448905601784759, 0.000000000000000000 ) ) ;
#19935 = CARTESIAN_POINT ( 'NONE',  ( -10.20829729246298889, 386.3698905765656377, 7.653668647301790529 ) ) ;
#19936 = CARTESIAN_POINT ( 'NONE',  ( -11.93348319268872793, 419.1823905683720000, -3.332260488124732856 ) ) ;
#19937 = CARTESIAN_POINT ( 'NONE',  ( -28.68588794268870146, 252.8698905683720000, -16.75240474999999307 ) ) ;
#19938 = CARTESIAN_POINT ( 'NONE',  ( -35.09675569278795848, 445.7448905683720000, 15.47720386886985366 ) ) ;
#19939 =( BOUNDED_CURVE ( )  B_SPLINE_CURVE ( 2, ( #2223, #19654, #14917, #1607, #8074, #15421, #3120, #3333, #13794, #6454, #6778, #16324, #8291, #13070, #20280, #18640, #14704 ),
 .UNSPECIFIED., .F., .T. ) 
 B_SPLINE_CURVE_WITH_KNOTS ( ( 3, 2, 2, 2, 2, 2, 2, 2, 3 ),
 ( 0.6875000000000002220, 0.6894531250000002220, 0.6914062500000002220, 0.6933593750000002220, 0.6953125000000002220, 0.6972656250000002220, 0.6992187500000002220, 0.7011718750000002220, 0.7031250000000002220 ),
 .UNSPECIFIED. ) 
 CURVE ( )  GEOMETRIC_REPRESENTATION_ITEM ( )  RATIONAL_B_SPLINE_CURVE ( ( 0.9999999999999977796, 0.9807852804032326510, 1.000000000000000000, 0.9807852804032304306, 1.000000000000000000, 0.9807852804032304306, 1.000000000000000000, 0.9807852804032304306, 1.000000000000000000, 0.9807852804032304306, 1.000000000000000000, 0.9807852804032304306, 1.000000000000000000, 0.9807852804032304306, 1.000000000000000000, 0.9807852804032282101, 1.000000000000002220 ) ) 
 REPRESENTATION_ITEM ( '' )  );
#19940 = CARTESIAN_POINT ( 'NONE',  ( 166.5371561215023348, 610.7448905601785327, -6.352526299242174268 ) ) ;
#19941 = EDGE_CURVE ( 'NONE', #2829, #12300, #7021, .T. ) ;
#19942 = CARTESIAN_POINT ( 'NONE',  ( -17.35679799567829207, 365.4323905765656377, 16.95518130045146421 ) ) ;
#19943 = CARTESIAN_POINT ( 'NONE',  ( 35.96497763894178945, 230.5765313837437418, 40.00000000000000000 ) ) ;
#19944 = DIRECTION ( 'NONE',  ( -1.232945044042657126E-32, 9.855701800883825964E-17, -1.000000000000000000 ) ) ;
#19945 = CARTESIAN_POINT ( 'NONE',  ( -20.54277306141295867, 585.7448905601785327, 49.33244044267773631 ) ) ;
#19946 = CARTESIAN_POINT ( 'NONE',  ( -48.68588794268863040, 491.6823905765656946, -3.978247347593371508 ) ) ;
#19947 = CARTESIAN_POINT ( 'NONE',  ( -44.16309181155858710, 504.7448905683720000, -6.410867750099231266 ) ) ;
#19948 = VECTOR ( 'NONE', #6950, 1000.000000000000000 ) ;
#19949 = DIRECTION ( 'NONE',  ( 0.9510565162951536422, 1.133459776540192910E-16, -0.3090169943749473958 ) ) ;
#19950 = LINE ( 'NONE', #8473, #12426 ) ;
#19951 = CARTESIAN_POINT ( 'NONE',  ( -47.16347859291445133, 417.8698905601784759, 7.653668647301805628 ) ) ;
#19952 =( REPRESENTATION_RELATIONSHIP ('NONE','NONE', #1888, #4076 ) REPRESENTATION_RELATIONSHIP_WITH_TRANSFORMATION ( #18732 )SHAPE_REPRESENTATION_RELATIONSHIP( ) );
#19953 = CIRCLE ( 'NONE', #9224, 22.72497359561857877 ) ;
#19954 = CARTESIAN_POINT ( 'NONE',  ( -22.27502019258949417, 412.2448905683720568, -15.47720386886985544 ) ) ;
#19955 = CARTESIAN_POINT ( 'NONE',  ( -48.68588794268874409, 588.2448905601785327, 2.449293598294706907E-15 ) ) ;
#19956 = CARTESIAN_POINT ( 'NONE',  ( -42.88789093042841927, 234.4323905683720284, -9.489475012073736337 ) ) ;
#19957 = CARTESIAN_POINT ( 'NONE',  ( -11.93348319268872260, 368.5573905683720568, 3.332260488124728415 ) ) ;
#19958 = ORIENTED_EDGE ( 'NONE', *, *, #12878, .T. ) ;
#19959 = CARTESIAN_POINT ( 'NONE',  ( -44.16309181155859420, 523.2448905683719431, -6.410867750099231266 ) ) ;
#19960 = ORIENTED_EDGE ( 'NONE', *, *, #10736, .T. ) ;
#19961 = CARTESIAN_POINT ( 'NONE',  ( -19.19641293061498999, 438.8073905683720000, 14.20200298773971426 ) ) ;
#19962 = CARTESIAN_POINT ( 'NONE',  ( -11.93348319268874214, 529.1823905683719431, -3.332260488124732856 ) ) ;
#19963 = ORIENTED_EDGE ( 'NONE', *, *, #11546, .T. ) ;
#19964 = CARTESIAN_POINT ( 'NONE',  ( -10.20829729246299422, 431.6198905601785327, 7.653668647301790529 ) ) ;
#19965 = CARTESIAN_POINT ( 'NONE',  ( -35.09675569278795848, 481.9948905683720000, -15.47720386886985544 ) ) ;
#19966 = ORIENTED_EDGE ( 'NONE', *, *, #2184, .F. ) ;
#19967 = CARTESIAN_POINT ( 'NONE',  ( -28.68588794268872988, 496.3698905683720568, 16.75240474999999307 ) ) ;
#19968 = CARTESIAN_POINT ( 'NONE',  ( -17.74224102826533311, 46.24521970153912065, -48.38107137947394421 ) ) ;
#19969 = CARTESIAN_POINT ( 'NONE',  ( -11.73070664223725856, 427.9323905765656377, -11.32908994701042715 ) ) ;
#19970 = CARTESIAN_POINT ( 'NONE',  ( 0.000000000000000000, 0.000000000000000000, 6.500000000000000000 ) ) ;
#19971 = CARTESIAN_POINT ( 'NONE',  ( 2.416697501590669095, 172.9933428177121471, 45.00000000000000000 ) ) ;
#19972 = CARTESIAN_POINT ( 'NONE',  ( -48.68588794268887909, 452.3073905765655809, 3.978247347592742678 ) ) ;
#19973 = CARTESIAN_POINT ( 'NONE',  ( 6.416697501590670427, 172.9933428177121471, 49.99999999999999289 ) ) ;
#19974 = DIRECTION ( 'NONE',  ( -1.000000000000000000, 0.000000000000000000, -0.000000000000000000 ) ) ;
#19975 = SURFACE_STYLE_FILL_AREA ( #13388 ) ;
#19976 = CARTESIAN_POINT ( 'NONE',  ( -8.685887942688713892, 223.9102039777116886, 2.449293598294704541E-15 ) ) ;
#19977 = CARTESIAN_POINT ( 'NONE',  ( -45.43829269268869808, 295.0573905683720000, -3.332260488124726194 ) ) ;
#19978 = CARTESIAN_POINT ( 'NONE',  ( -11.73070664223726745, 531.3073905601785327, 11.32908994701042005 ) ) ;
#19979 = CARTESIAN_POINT ( 'NONE',  ( -48.68588794268870146, 277.5573905601784190, 3.978247347593168115 ) ) ;
#19980 = CARTESIAN_POINT ( 'NONE',  ( -32.69826294449585191, 51.81229826077375833, -49.43888307834195928 ) ) ;
#19981 = CARTESIAN_POINT ( 'NONE',  ( -35.09675569278793716, 283.4948905683720000, -15.47720386886985544 ) ) ;
#19982 = ADVANCED_FACE ( 'NONE', ( #8222 ), #14851, .T. ) ;
#19983 = DIRECTION ( 'NONE',  ( -0.000000000000000000, -0.000000000000000000, -1.000000000000000000 ) ) ;
#19984 = CARTESIAN_POINT ( 'NONE',  ( -11.93348319268873858, 510.0573905683719431, 3.332260488124728859 ) ) ;
#19985 = ORIENTED_EDGE ( 'NONE', *, *, #7877, .T. ) ;
#19986 = CARTESIAN_POINT ( 'NONE',  ( -45.43829269268872650, 475.3698905683720568, 0.000000000000000000 ) ) ;
#19987 = EDGE_CURVE ( 'NONE', #7807, #4231, #4987, .T. ) ;
#19988 = CARTESIAN_POINT ( 'NONE',  ( -40.01497788969914637, 410.4323905765655809, -16.95518130045146421 ) ) ;
#19989 = CARTESIAN_POINT ( 'NONE',  ( -35.09675569278793006, 261.9948905683720000, -15.47720386886985544 ) ) ;
#19990 = ORIENTED_EDGE ( 'NONE', *, *, #6980, .T. ) ;
#19991 = CARTESIAN_POINT ( 'NONE',  ( 0.06682554136338486606, -6.264794173742287420, -2.149058192116898081 ) ) ;
#19992 = VECTOR ( 'NONE', #4176, 1000.000000000000000 ) ;
#19993 = CARTESIAN_POINT ( 'NONE',  ( -14.48388495494898720, 269.4323905683720568, 9.489475012073731008 ) ) ;
#19994 = CARTESIAN_POINT ( 'NONE',  ( -16.84014894278197616, 241.6198905683720284, -11.84573899990672707 ) ) ;
#19995 = CARTESIAN_POINT ( 'NONE',  ( -48.68588794268869435, 241.6823905765655809, -3.978247347593158345 ) ) ;
#19996 = CARTESIAN_POINT ( 'NONE',  ( -48.68588794268870146, 307.2448905601784759, 0.000000000000000000 ) ) ;
#19997 = CARTESIAN_POINT ( 'NONE',  ( -36.33955658999049376, 235.3698905601784759, -18.47759065022572855 ) ) ;
#19998 = CARTESIAN_POINT ( 'NONE',  ( -42.88789093042842637, 274.8073905683720000, 9.489475012073736337 ) ) ;
#19999 = CARTESIAN_POINT ( 'NONE',  ( -14.48388495494899608, 349.4323905683720000, 9.489475012073732785 ) ) ;
#20000 = VECTOR ( 'NONE', #11568, 999.9999999999998863 ) ;
#20001 = DIRECTION ( 'NONE',  ( 0.000000000000000000, 0.000000000000000000, 1.000000000000000000 ) ) ;
#20002 = LINE ( 'NONE', #9719, #7272 ) ;
#20003 = AXIS2_PLACEMENT_3D ( 'NONE', #8571, #15194, #11720 ) ;
#20004 = EDGE_CURVE ( 'NONE', #13368, #20443, #15681, .T. ) ;
#20005 = CARTESIAN_POINT ( 'NONE',  ( -42.88789093042844058, 424.8073905683720000, 9.489475012073736337 ) ) ;
#20006 = DIRECTION ( 'NONE',  ( 0.000000000000000000, -0.8660254037844380415, 0.5000000000000011102 ) ) ;
#20007 = VERTEX_POINT ( 'NONE', #9953 ) ;
#20008 = CARTESIAN_POINT ( 'NONE',  ( -36.33955658999052218, 399.1198905601784759, 18.47759065022572500 ) ) ;
#20009 = VERTEX_POINT ( 'NONE', #6817 ) ;
#20010 = EDGE_LOOP ( 'NONE', ( #10253, #17620, #19109, #7681 ) ) ;
#20011 = EDGE_LOOP ( 'NONE', ( #15349, #6018, #4342, #8828, #9681 ) ) ;
#20012 = CARTESIAN_POINT ( 'NONE',  ( -11.93348319268874214, 530.3698905683720568, -2.051577885510841163E-15 ) ) ;
#20013 = VECTOR ( 'NONE', #17905, 1000.000000000000114 ) ;
#20014 = CARTESIAN_POINT ( 'NONE',  ( -36.33955658999050087, 295.3698905601784759, -18.47759065022572855 ) ) ;
#20015 = CARTESIAN_POINT ( 'NONE',  ( 65.85920792673738333, 160.1716627696692683, 40.00000000000000000 ) ) ;
#20016 = ORIENTED_EDGE ( 'NONE', *, *, #14468, .T. ) ;
#20017 = CARTESIAN_POINT ( 'NONE',  ( -13.20868407381885312, 319.7448905683720000, 6.410867750099229490 ) ) ;
#20018 = CARTESIAN_POINT ( 'NONE',  ( -25.35362745456399125, 361.0573905683720000, -16.75240474999999307 ) ) ;
#20019 = CARTESIAN_POINT ( 'NONE',  ( -42.88789093042843348, 372.9323905683720568, -9.489475012073734561 ) ) ;
#20020 = AXIS2_PLACEMENT_3D ( 'NONE', #12761, #19351, #18046 ) ;
#20021 = EDGE_CURVE ( 'NONE', #16325, #18084, #12094, .T. ) ;
#20022 = CARTESIAN_POINT ( 'NONE',  ( -32.66413529028186957, 304.1823905765656377, 19.99999999999999289 ) ) ;
#20023 = CARTESIAN_POINT ( 'NONE',  ( -43.68588794268869435, 200.1437886375728965, -2.037320803886357560E-15 ) ) ;
#20024 = CARTESIAN_POINT ( 'NONE',  ( -22.27502019258947641, 260.7448905683720000, -15.47720386886985544 ) ) ;
#20025 = CARTESIAN_POINT ( 'NONE',  ( -48.68588794268880804, 437.5573905601785327, 3.978247347592954952 ) ) ;
#20026 = CARTESIAN_POINT ( 'NONE',  ( -22.27502019258949417, 422.2448905683720568, -15.47720386886985544 ) ) ;
#20027 = CARTESIAN_POINT ( 'NONE',  ( -24.92302309252174197, 45.61007917770206888, 122.4907538390011439 ) ) ;
#20028 = CARTESIAN_POINT ( 'NONE',  ( -48.68588794268867304, 516.9323905601784190, -3.978247347593264927 ) ) ;
#20029 = CARTESIAN_POINT ( 'NONE',  ( 0.5805565836007642311, -3.752776749732576356, -6.499999999999999112 ) ) ;
#20030 = LINE ( 'NONE', #8976, #14971 ) ;
#20031 = EDGE_CURVE ( 'NONE', #4181, #14447, #6979, .T. ) ;
#20032 = CARTESIAN_POINT ( 'NONE',  ( -22.27502019258949062, 486.9948905683720568, 15.47720386886985189 ) ) ;
#20033 = VERTEX_POINT ( 'NONE', #2284 ) ;
#20034 = CARTESIAN_POINT ( 'NONE',  ( -8.685887942688735208, 472.2448905601784759, -2.449293598294705724E-15 ) ) ;
#20035 = CARTESIAN_POINT ( 'NONE',  ( -44.16309181155856578, 313.2448905683720000, -6.410867750099231266 ) ) ;
#20036 = ORIENTED_EDGE ( 'NONE', *, *, #13730, .T. ) ;
#20037 = CARTESIAN_POINT ( 'NONE',  ( 21.30000000000000071, 0.000000000000000000, 3.309499999999999886 ) ) ;
#20038 = ORIENTED_EDGE ( 'NONE', *, *, #8287, .F. ) ;
#20039 = CARTESIAN_POINT ( 'NONE',  ( -28.68588794268874054, 573.2448905601785327, 0.000000000000000000 ) ) ;
#20040 = CARTESIAN_POINT ( 'NONE',  ( -11.93348319268872437, 390.0573905683720568, 3.332260488124728859 ) ) ;
#20041 = DIRECTION ( 'NONE',  ( -0.000000000000000000, 1.000000000000000000, -0.000000000000000000 ) ) ;
#20042 = CARTESIAN_POINT ( 'NONE',  ( -41.83569717483972994, 326.0737056351150613, -24.99999999999998934 ) ) ;
#20043 = CARTESIAN_POINT ( 'NONE',  ( -40.53162694259544452, 432.6198905683720000, -11.84573899990672707 ) ) ;
#20044 = CARTESIAN_POINT ( 'NONE',  ( -14.48388495494898720, 261.3073905683720568, -9.489475012073736337 ) ) ;
#20045 = VECTOR ( 'NONE', #7496, 1000.000000000000000 ) ;
#20046 = CARTESIAN_POINT ( 'NONE',  ( -35.09675569278795138, 431.9948905683720568, -15.47720386886985544 ) ) ;
#20047 = APPLICATION_PROTOCOL_DEFINITION ( 'draft international standard', 'automotive_design', 1998, #20085 ) ;
#20048 = CIRCLE ( 'NONE', #21079, 125.0000000000000000 ) ;
#20049 = DIRECTION ( 'NONE',  ( 0.000000000000000000, 0.000000000000000000, 1.000000000000000000 ) ) ;
#20050 = CARTESIAN_POINT ( 'NONE',  ( -17.35679799567829207, 355.4323905765655809, 16.95518130045146421 ) ) ;
#20051 = CYLINDRICAL_SURFACE ( 'NONE', #14491, 6.500000000000000888 ) ;
#20052 = CARTESIAN_POINT ( 'NONE',  ( -28.68588794268874054, 573.2448905601785327, 0.000000000000000000 ) ) ;
#20053 = CARTESIAN_POINT ( 'NONE',  ( -25.35362745456397704, 326.6823905683720568, 16.75240474999998952 ) ) ;
#20054 = CARTESIAN_POINT ( 'NONE',  ( 52.60622592008805043, 10.52886280891152104, -151.0302712373927250 ) ) ;
#20055 = CARTESIAN_POINT ( 'NONE',  ( -14.48388495494901029, 479.4323905683720568, 9.489475012073732785 ) ) ;
#20057 = PLANE ( 'NONE',  #19586 ) ;
#20056 =( GEOMETRIC_REPRESENTATION_CONTEXT ( 3 ) GLOBAL_UNCERTAINTY_ASSIGNED_CONTEXT ( ( #11591 ) ) GLOBAL_UNIT_ASSIGNED_CONTEXT ( ( #14527, #21010, #9529 ) ) REPRESENTATION_CONTEXT ( 'NONE', 'WORKASPACE' ) );
#20058 = LINE ( 'NONE', #3405, #16289 ) ;
#20059 = CARTESIAN_POINT ( 'NONE',  ( -17.35679799567829562, 420.6823905601784190, 16.95518130045146421 ) ) ;
#20060 = CARTESIAN_POINT ( 'NONE',  ( -45.43829269268870519, 385.0573905683720000, -3.332260488124726194 ) ) ;
#20061 = CIRCLE ( 'NONE', #15927, 6.500000000000000888 ) ;
#20062 = CARTESIAN_POINT ( 'NONE',  ( -22.30770786884144741, 45.31613216062291372, -122.9933582338429687 ) ) ;
#20063 = EDGE_CURVE ( 'NONE', #534, #1580, #7342, .T. ) ;
#20064 = CARTESIAN_POINT ( 'NONE',  ( -45.43829269268869098, 235.6823905683720284, 3.332260488124734632 ) ) ;
#20065 = CARTESIAN_POINT ( 'NONE',  ( -28.68588794268871567, 361.3698905683720568, -16.75240474999999307 ) ) ;
#20066 = EDGE_CURVE ( 'NONE', #14788, #1090, #2178, .T. ) ;
#20067 = ORIENTED_EDGE ( 'NONE', *, *, #4137, .T. ) ;
#20068 = CARTESIAN_POINT ( 'NONE',  ( -14.48388495494901917, 529.8073905683720568, -9.489475012073736337 ) ) ;
#20069 = EDGE_LOOP ( 'NONE', ( #20728, #10070, #8378, #3457 ) ) ;
#20070 = CARTESIAN_POINT ( 'NONE',  ( -32.01814843081344719, 443.1823905683720568, -16.75240474999999307 ) ) ;
#20071 = CARTESIAN_POINT ( 'NONE',  ( -32.01814843081346851, 526.0573905683720568, 16.75240474999999307 ) ) ;
#20072 = ADVANCED_FACE ( 'NONE', ( #8469 ), #13153, .T. ) ;
#20073 = ORIENTED_EDGE ( 'NONE', *, *, #7215, .T. ) ;
#20074 = CARTESIAN_POINT ( 'NONE',  ( -47.16347859291445133, 427.8698905601784759, 7.653668647301805628 ) ) ;
#20075 = CARTESIAN_POINT ( 'NONE',  ( -19.19641293061499709, 480.4323905683720568, -14.20200298773971603 ) ) ;
#20076 = ORIENTED_EDGE ( 'NONE', *, *, #10354, .F. ) ;
#20077 = CARTESIAN_POINT ( 'NONE',  ( -13.20868407381887621, 489.4948905683720568, -6.410867750099233042 ) ) ;
#20078 = CARTESIAN_POINT ( 'NONE',  ( -20.71406170972610639, 45.37974668544075740, -48.96689081729963533 ) ) ;
#20079 = VECTOR ( 'NONE', #3739, 1000.000000000000000 ) ;
#20081 = VECTOR ( 'NONE', #3271, 1000.000000000000000 ) ;
#20080 = CARTESIAN_POINT ( 'NONE',  ( -14.54375231895777887, 428.2448905765656377, -14.14213562373094746 ) ) ;
#20082 = DIRECTION ( 'NONE',  ( 0.9362971185447988010, -0.000000000000000000, 0.3512089204514987628 ) ) ;
#20083 = DIRECTION ( 'NONE',  ( 1.191790137725560488E-16, -1.000000000000000000, -0.000000000000000000 ) ) ;
#20084 = DIRECTION ( 'NONE',  ( 1.000000000000000000, 1.191790137725560488E-16, 0.000000000000000000 ) ) ;
#20085 = APPLICATION_CONTEXT ( 'automotive_design' ) ;
#20086 = DIRECTION ( 'NONE',  ( -1.000000000000000000, -0.000000000000000000, -0.000000000000000000 ) ) ;
#20087 = CARTESIAN_POINT ( 'NONE',  ( 0.000000000000000000, 0.000000000000000000, -6.499999999999999112 ) ) ;
#20088 = CARTESIAN_POINT ( 'NONE',  ( -42.87299489053027912, 204.0036020648173292, -4.871053504435129078 ) ) ;
#20089 = CARTESIAN_POINT ( 'NONE',  ( -42.88789093042842637, 304.4323905683720000, -9.489475012073736337 ) ) ;
#20090 = DIRECTION ( 'NONE',  ( -0.000000000000000000, -0.000000000000000000, 1.000000000000000000 ) ) ;
#20091 = CARTESIAN_POINT ( 'NONE',  ( -21.03221929538691271, 264.1198905601784759, -18.47759065022572855 ) ) ;
#20092 = CARTESIAN_POINT ( 'NONE',  ( -31.26501780185373391, 205.1437886375728965, 5.000000000000001776 ) ) ;
#20093 = CARTESIAN_POINT ( 'NONE',  ( -25.35362745456398059, 282.5573905683720568, -16.75240474999999307 ) ) ;
#20094 = ORIENTED_EDGE ( 'NONE', *, *, #5960, .T. ) ;
#20095 = CARTESIAN_POINT ( 'NONE',  ( -1.025382690249029949, 160.1716627696692683, 25.00000000000000000 ) ) ;
#20096 = AXIS2_PLACEMENT_3D ( 'NONE', #14517, #21101, #4659 ) ;
#20097 = CARTESIAN_POINT ( 'NONE',  ( -19.19641293061499709, 508.8073905683720000, 14.20200298773971426 ) ) ;
#20098 = ORIENTED_EDGE ( 'NONE', *, *, #5468, .T. ) ;
#20099 = CARTESIAN_POINT ( 'NONE',  ( -25.35362745456399125, 458.1823905683720000, 16.75240474999998952 ) ) ;
#20100 = CYLINDRICAL_SURFACE ( 'NONE', #8290, 19.99999999999999645 ) ;
#20101 = CARTESIAN_POINT ( 'NONE',  ( -28.68588794268870501, 261.3698905683720000, -16.75240474999999307 ) ) ;
#20102 = ORIENTED_EDGE ( 'NONE', *, *, #6116, .T. ) ;
#20103 = CARTESIAN_POINT ( 'NONE',  ( 0.2578475836320768821, -6.890627091270383531, -1.065083781909174743 ) ) ;
#20104 = CARTESIAN_POINT ( 'NONE',  ( -16.84014894278197971, 271.6198905683720568, -11.84573899990672707 ) ) ;
#20105 = CARTESIAN_POINT ( 'NONE',  ( -25.35362745456396638, 238.1823905683720852, 16.75240474999998952 ) ) ;
#20106 = CARTESIAN_POINT ( 'NONE',  ( -8.685887942688893304, 311.9323905601784190, 3.978247347593586447 ) ) ;
#20107 = FACE_OUTER_BOUND ( 'NONE', #11137, .T. ) ;
#20108 = CARTESIAN_POINT ( 'NONE',  ( -28.68588794268870501, 261.3698905683720000, -16.75240474999999307 ) ) ;
#20109 = AXIS2_PLACEMENT_3D ( 'NONE', #11644, #8498, #3738 ) ;
#20110 = CARTESIAN_POINT ( 'NONE',  ( -22.27502019258948707, 352.2448905683720000, -15.47720386886985544 ) ) ;
#20111 = CARTESIAN_POINT ( 'NONE',  ( -10.20829729246300310, 502.8698905601784759, -7.653668647301794969 ) ) ;
#20112 = EDGE_CURVE ( 'NONE', #11812, #9678, #11010, .T. ) ;
#20113 = CARTESIAN_POINT ( 'NONE',  ( -38.17536295476246266, 412.3073905683720000, -14.20200298773971426 ) ) ;
#20114 = CARTESIAN_POINT ( 'NONE',  ( -40.01497788969913927, 340.4323905765656946, -16.95518130045146421 ) ) ;
#20115 = ORIENTED_EDGE ( 'NONE', *, *, #3329, .F. ) ;
#20116 = CARTESIAN_POINT ( 'NONE',  ( -40.01497788969914637, 415.6823905601785327, -16.95518130045146421 ) ) ;
#20117 = ORIENTED_EDGE ( 'NONE', *, *, #13954, .T. ) ;
#20118 = CARTESIAN_POINT ( 'NONE',  ( -71.26501780185373036, 130.1716627696692683, 1.734723475976807094E-15 ) ) ;
#20119 = ORIENTED_EDGE ( 'NONE', *, *, #1382, .T. ) ;
#20120 = VERTEX_POINT ( 'NONE', #7129 ) ;
#20121 = CARTESIAN_POINT ( 'NONE',  ( -28.68588794268873343, 527.8698905683720568, 16.75240474999999307 ) ) ;
#20122 = CARTESIAN_POINT ( 'NONE',  ( -17.35679799567828141, 280.6823905601784190, 16.95518130045146421 ) ) ;
#20123 = CARTESIAN_POINT ( 'NONE',  ( -43.67243589781771362, 210.1033101532991338, -0.6559853996653195463 ) ) ;
#20124 = VECTOR ( 'NONE', #18165, 1000.000000000000000 ) ;
#20125 = ORIENTED_EDGE ( 'NONE', *, *, #7023, .F. ) ;
#20126 = CARTESIAN_POINT ( 'NONE',  ( -22.27502019258948351, 332.2448905683720568, -15.47720386886985544 ) ) ;
#20127 = ORIENTED_EDGE ( 'NONE', *, *, #5457, .F. ) ;
#20128 = CARTESIAN_POINT ( 'NONE',  ( -19.19641293061498288, 367.3073905683720000, 14.20200298773971426 ) ) ;
#20129 = CARTESIAN_POINT ( 'NONE',  ( -42.88789093042843348, 362.9323905683720568, -9.489475012073734561 ) ) ;
#20130 = EDGE_CURVE ( 'NONE', #20205, #13969, #16372, .T. ) ;
#20131 = CARTESIAN_POINT ( 'NONE',  ( -45.64106924314017988, 311.0573905765656377, -11.32908994701042715 ) ) ;
#20132 = CARTESIAN_POINT ( 'NONE',  ( 292.4526463419396691, 308.2087638784415162, -40.00000000000000000 ) ) ;
#20133 = CARTESIAN_POINT ( 'NONE',  ( -28.68588794268870501, 261.3698905683720000, -16.75240474999999307 ) ) ;
#20134 = DIRECTION ( 'NONE',  ( 1.000000000000000000, 0.000000000000000000, 0.000000000000000000 ) ) ;
#20135 = AXIS2_PLACEMENT_3D ( 'NONE', #6205, #4693, #6313 ) ;
#20136 = CARTESIAN_POINT ( 'NONE',  ( -16.84014894278199748, 421.6198905683720000, -11.84573899990672707 ) ) ;
#20137 = DIRECTION ( 'NONE',  ( -1.191790137725560488E-16, 1.000000000000000000, -0.000000000000000000 ) ) ;
#20138 = CARTESIAN_POINT ( 'NONE',  ( -17.35679799567829562, 353.8073905601785327, -16.95518130045146421 ) ) ;
#20139 = CARTESIAN_POINT ( 'NONE',  ( -47.16347859291443712, 272.6198905765655809, 7.653668647301805628 ) ) ;
#20140 = CARTESIAN_POINT ( 'NONE',  ( -32.66413529028187668, 409.4323905601784759, 19.99999999999999289 ) ) ;
#20141 = CARTESIAN_POINT ( 'NONE',  ( -42.88789093042843348, 336.3073905683720568, 9.489475012073736337 ) ) ;
#20142 = CARTESIAN_POINT ( 'NONE',  ( -28.68588794268872277, 456.3698905683720000, 16.75240474999999307 ) ) ;
#20143 = EDGE_LOOP ( 'NONE', ( #3746, #2609 ) ) ;
#20144 = CARTESIAN_POINT ( 'NONE',  ( -48.68588794268872277, 456.9323905601784190, -3.978247347593158345 ) ) ;
#20145 = CARTESIAN_POINT ( 'NONE',  ( -28.68588794268870856, 301.3698905683720568, -16.75240474999999307 ) ) ;
#20146 = ADVANCED_FACE ( 'NONE', ( #13755 ), #12231, .F. ) ;
#20147 = ORIENTED_EDGE ( 'NONE', *, *, #15708, .F. ) ;
#20148 = EDGE_LOOP ( 'NONE', ( #15768, #5499, #9750, #17691, #15523, #4261 ) ) ;
#20149 = CYLINDRICAL_SURFACE ( 'NONE', #13984, 19.99999999999999645 ) ;
#20150 = CIRCLE ( 'NONE', #18743, 220.7252770684331438 ) ;
#20151 = CARTESIAN_POINT ( 'NONE',  ( -14.48388495494899963, 379.4323905683720568, 9.489475012073731008 ) ) ;
#20152 = DIRECTION ( 'NONE',  ( 0.000000000000000000, 1.000000000000000000, -0.000000000000000000 ) ) ;
#20153 = CARTESIAN_POINT ( 'NONE',  ( 65.85920792673738333, 160.1716627696692683, -20.00000000000000355 ) ) ;
#20154 = CARTESIAN_POINT ( 'NONE',  ( -35.09675569278795848, 425.7448905683720000, 15.47720386886985366 ) ) ;
#20155 = CARTESIAN_POINT ( 'NONE',  ( -11.93348319268871194, 270.0573905683719431, 3.332260488124728415 ) ) ;
#20156 = CARTESIAN_POINT ( 'NONE',  ( -38.17536295476245556, 425.4323905683719431, 14.20200298773971781 ) ) ;
#20157 = APPLICATION_PROTOCOL_DEFINITION ( 'draft international standard', 'automotive_design', 1998, #1706 ) ;
#20158 = CARTESIAN_POINT ( 'NONE',  ( 0.000000000000000000, 31.85652257517428865, 0.000000000000000000 ) ) ;
#20159 = ADVANCED_FACE ( 'NONE', ( #5725 ), #20341, .F. ) ;
#20160 = CARTESIAN_POINT ( 'NONE',  ( -24.70764059509555111, 364.8073905765656377, 19.99999999999998934 ) ) ;
#20161 = CARTESIAN_POINT ( 'NONE',  ( -24.70764059509554755, 274.4323905601784759, -19.99999999999999289 ) ) ;
#20162 = CARTESIAN_POINT ( 'NONE',  ( -44.16309181155856578, 323.2448905683720000, -6.410867750099231266 ) ) ;
#20163 = CARTESIAN_POINT ( 'NONE',  ( -45.43829269268873361, 533.8698905683720568, 0.000000000000000000 ) ) ;
#20164 = CARTESIAN_POINT ( 'NONE',  ( -28.68588794268872633, 477.8698905683720568, 16.75240474999999307 ) ) ;
#20165 = VECTOR ( 'NONE', #7569, 1000.000000000000000 ) ;
#20166 = CARTESIAN_POINT ( 'NONE',  ( -24.70764059509555821, 434.8073905765656377, 19.99999999999998934 ) ) ;
#20167 = DIRECTION ( 'NONE',  ( -1.000000000000000000, -0.000000000000000000, -0.000000000000000000 ) ) ;
#20168 = DIRECTION ( 'NONE',  ( 0.000000000000000000, 0.000000000000000000, -1.000000000000000000 ) ) ;
#20169 = AXIS2_PLACEMENT_3D ( 'NONE', #7506, #7400, #17679 ) ;
#20170 = CARTESIAN_POINT ( 'NONE',  ( -42.88789093042844058, 396.3073905683719431, 9.489475012073736337 ) ) ;
#20171 = DIRECTION ( 'NONE',  ( -1.191790137725560488E-16, 1.000000000000000000, -0.000000000000000000 ) ) ;
#20172 = CARTESIAN_POINT ( 'NONE',  ( -10.20829729246300488, 522.8698905601785327, -7.653668647301794969 ) ) ;
#20173 = CARTESIAN_POINT ( 'NONE',  ( -11.93348319268872260, 359.1823905683720000, -3.332260488124732856 ) ) ;
#20174 = ORIENTED_EDGE ( 'NONE', *, *, #2670, .T. ) ;
#20175 = CARTESIAN_POINT ( 'NONE',  ( -22.27502019258950483, 520.7448905683720568, -15.47720386886985544 ) ) ;
#20176 = ORIENTED_EDGE ( 'NONE', *, *, #9538, .F. ) ;
#20177 = CARTESIAN_POINT ( 'NONE',  ( -45.43829269268872650, 524.1823905683720568, 3.332260488124734632 ) ) ;
#20178 = ORIENTED_EDGE ( 'NONE', *, *, #15327, .T. ) ;
#20179 = CARTESIAN_POINT ( 'NONE',  ( -14.48388495494901029, 477.9323905683721136, 9.489475012073732785 ) ) ;
#20180 = ORIENTED_EDGE ( 'NONE', *, *, #4332, .T. ) ;
#20181 = CARTESIAN_POINT ( 'NONE',  ( -45.43829269268872650, 483.8698905683720568, 0.000000000000000000 ) ) ;
#20182 = CIRCLE ( 'NONE', #2952, 6.500000000000000888 ) ;
#20183 = CARTESIAN_POINT ( 'NONE',  ( -14.54375231895777709, 418.2448905765655809, -14.14213562373094746 ) ) ;
#20184 = CARTESIAN_POINT ( 'NONE',  ( -28.68588794268872633, 474.4948905765656377, 19.99999999999999289 ) ) ;
#20185 = CARTESIAN_POINT ( 'NONE',  ( -162.2727221670389781, 10.52886280891152104, -20.57735571454641033 ) ) ;
#20186 = LINE ( 'NONE', #2128, #16021 ) ;
#20187 = PLANE ( 'NONE',  #4245 ) ;
#20188 = DIRECTION ( 'NONE',  ( -9.855701800883827197E-17, 1.000000000000000000, -0.000000000000000000 ) ) ;
#20189 = CARTESIAN_POINT ( 'NONE',  ( -28.68588794268870501, 297.8698905683720000, 16.75240474999999307 ) ) ;
#20190 = CARTESIAN_POINT ( 'NONE',  ( -47.16347859291446554, 527.8698905601784190, 7.653668647301805628 ) ) ;
#20191 = CARTESIAN_POINT ( 'NONE',  ( -45.43829269268871229, 445.0573905683720000, -3.332260488124726194 ) ) ;
#20192 = CARTESIAN_POINT ( 'NONE',  ( -32.89690641512254388, 52.24437994842455879, -49.42213772442809727 ) ) ;
#20193 =( BOUNDED_CURVE ( )  B_SPLINE_CURVE ( 2, ( #8239, #5320, #14869, #8349, #14973, #13347, #799, #17228, #5534, #13992, #688, #12139, #12249, #7255, #18725, #8991, #903 ),
 .UNSPECIFIED., .F., .T. ) 
 B_SPLINE_CURVE_WITH_KNOTS ( ( 3, 2, 2, 2, 2, 2, 2, 2, 3 ),
 ( 0.5000000000000002220, 0.5019531250000002220, 0.5039062500000002220, 0.5058593750000002220, 0.5078125000000002220, 0.5097656250000002220, 0.5117187500000002220, 0.5136718750000002220, 0.5156250000000002220 ),
 .UNSPECIFIED. ) 
 CURVE ( )  GEOMETRIC_REPRESENTATION_ITEM ( )  RATIONAL_B_SPLINE_CURVE ( ( 0.9999999999999977796, 0.9807852804032326510, 1.000000000000000000, 0.9807852804032304306, 1.000000000000000000, 0.9807852804032304306, 1.000000000000000000, 0.9807852804032304306, 1.000000000000000000, 0.9807852804032304306, 1.000000000000000000, 0.9807852804032304306, 1.000000000000000000, 0.9807852804032304306, 1.000000000000000000, 0.9807852804032282101, 1.000000000000002220 ) ) 
 REPRESENTATION_ITEM ( '' )  );
#20194 = CARTESIAN_POINT ( 'NONE',  ( -40.53162694259542320, 264.1198905683720568, -11.84573899990672707 ) ) ;
#20195 = EDGE_CURVE ( 'NONE', #13560, #13932, #10010, .T. ) ;
#20196 = ORIENTED_EDGE ( 'NONE', *, *, #3336, .F. ) ;
#20197 = CARTESIAN_POINT ( 'NONE',  ( 20.42502041961814641, 160.1716627696692683, 40.00000000000000000 ) ) ;
#20198 = CARTESIAN_POINT ( 'NONE',  ( -22.27502019258949417, 498.4948905683720568, 15.47720386886985189 ) ) ;
#20199 = ADVANCED_FACE ( 'NONE', ( #14610 ), #7670, .T. ) ;
#20200 = EDGE_CURVE ( 'NONE', #12831, #5170, #19040, .T. ) ;
#20201 = VERTEX_POINT ( 'NONE', #12763 ) ;
#20202 = CARTESIAN_POINT ( 'NONE',  ( -25.35362745456400546, 472.5573905683720568, -16.75240474999999307 ) ) ;
#20203 = CARTESIAN_POINT ( 'NONE',  ( 0.000000000000000000, 0.000000000000000000, 0.000000000000000000 ) ) ;
#20204 = CARTESIAN_POINT ( 'NONE',  ( -40.53162694259542320, 255.1198905683720284, 11.84573899990672885 ) ) ;
#20205 = VERTEX_POINT ( 'NONE', #14297 ) ;
#20206 = LINE ( 'NONE', #217, #4533 ) ;
#20207 = CARTESIAN_POINT ( 'NONE',  ( -25.35362745456396993, 268.1823905683720000, 16.75240474999998952 ) ) ;
#20208 = CARTESIAN_POINT ( 'NONE',  ( -11.73070664223724968, 391.3073905601784759, 11.32908994701042005 ) ) ;
#20209 = CARTESIAN_POINT ( 'NONE',  ( -25.35362745456396638, 248.1823905683720568, 16.75240474999998952 ) ) ;
#20210 = ADVANCED_FACE ( 'NONE', ( #14185 ), #1185, .T. ) ;
#20211 = CARTESIAN_POINT ( 'NONE',  ( -14.54375231895775933, 310.9948905601784759, 14.14213562373094568 ) ) ;
#20212 = FACE_OUTER_BOUND ( 'NONE', #1363, .T. ) ;
#20213 = CARTESIAN_POINT ( 'NONE',  ( -45.43829269268869808, 273.5573905683720000, -3.332260488124726194 ) ) ;
#20214 = CARTESIAN_POINT ( 'NONE',  ( -32.01814843081344719, 353.1823905683720568, -16.75240474999999307 ) ) ;
#20215 = PLANE ( 'NONE',  #11961 ) ;
#20216 = CARTESIAN_POINT ( 'NONE',  ( -22.27502019258949417, 410.7448905683720568, -15.47720386886985544 ) ) ;
#20217 = DIRECTION ( 'NONE',  ( -1.000000000000000000, -0.000000000000000000, -0.000000000000000000 ) ) ;
#20218 = CARTESIAN_POINT ( 'NONE',  ( -8.685887942688726326, 402.5573905601784190, -3.978247347593165895 ) ) ;
#20219 = ORIENTED_EDGE ( 'NONE', *, *, #3878, .F. ) ;
#20220 = DIRECTION ( 'NONE',  ( -1.191790137725560488E-16, 1.000000000000000000, -0.000000000000000000 ) ) ;
#20221 = ORIENTED_EDGE ( 'NONE', *, *, #11250, .F. ) ;
#20222 = ORIENTED_EDGE ( 'NONE', *, *, #1749, .F. ) ;
#20223 = CARTESIAN_POINT ( 'NONE',  ( -25.35362745456399836, 518.1823905683720568, 16.75240474999998952 ) ) ;
#20224 = CARTESIAN_POINT ( 'NONE',  ( -8.685887942688713892, 291.9323905601784759, 3.978247347593161010 ) ) ;
#20225 = CARTESIAN_POINT ( 'NONE',  ( -36.33955658999050087, 320.1198905765656377, -18.47759065022572855 ) ) ;
#20226 = ORIENTED_EDGE ( 'NONE', *, *, #17994, .T. ) ;
#20227 = CARTESIAN_POINT ( 'NONE',  ( -11.93348319268871727, 330.0573905683720000, 3.332260488124728859 ) ) ;
#20228 = EDGE_LOOP ( 'NONE', ( #1004, #9786, #17065, #8094 ) ) ;
#20229 = CARTESIAN_POINT ( 'NONE',  ( -16.84014894278198327, 337.6198905683720000, 11.84573899990672530 ) ) ;
#20230 = CARTESIAN_POINT ( 'NONE',  ( -14.48388495494899963, 367.9323905683720000, 9.489475012073731008 ) ) ;
#20231 = CARTESIAN_POINT ( 'NONE',  ( -8.685887942688715668, 306.6823905765655809, 3.978247347593161010 ) ) ;
#20232 = DIRECTION ( 'NONE',  ( 0.9997392892938121722, 0.02283316540262222971, 0.000000000000000000 ) ) ;
#20233 = CARTESIAN_POINT ( 'NONE',  ( -35.09675569278794427, 275.7448905683720568, 15.47720386886985366 ) ) ;
#20234 = CARTESIAN_POINT ( 'NONE',  ( -43.68588794268869435, 200.1437886375728397, 0.3328713742805498588 ) ) ;
#20235 = CARTESIAN_POINT ( 'NONE',  ( -19.19641293061498999, 411.9323905683720000, -14.20200298773971603 ) ) ;
#20236 = CARTESIAN_POINT ( 'NONE',  ( -22.30770786884143675, 45.31613216062291372, 122.9933582338429687 ) ) ;
#20237 = DIRECTION ( 'NONE',  ( -0.000000000000000000, 0.000000000000000000, -1.000000000000000000 ) ) ;
#20238 = DIRECTION ( 'NONE',  ( 0.000000000000000000, -1.000000000000000000, 0.000000000000000000 ) ) ;
#20239 = CARTESIAN_POINT ( 'NONE',  ( -11.93348319268871727, 330.3698905683720000, -2.051577885510841163E-15 ) ) ;
#20240 = CARTESIAN_POINT ( 'NONE',  ( -38.17536295476246266, 465.4323905683720000, 14.20200298773971781 ) ) ;
#20241 = ORIENTED_EDGE ( 'NONE', *, *, #19009, .T. ) ;
#20242 = CARTESIAN_POINT ( 'NONE',  ( -24.70764059509556532, 470.0573905601784759, 19.99999999999998934 ) ) ;
#20243 = CARTESIAN_POINT ( 'NONE',  ( -45.43829269268869808, 284.1823905683720568, 3.332260488124734632 ) ) ;
#20244 = EDGE_CURVE ( 'NONE', #13932, #6110, #19295, .T. ) ;
#20245 = ORIENTED_EDGE ( 'NONE', *, *, #12935, .T. ) ;
#20246 = CARTESIAN_POINT ( 'NONE',  ( -35.86044580198795018, 223.9104597372275123, 18.66884633871304899 ) ) ;
#20247 = ORIENTED_EDGE ( 'NONE', *, *, #16571, .T. ) ;
#20248 = CYLINDRICAL_SURFACE ( 'NONE', #3946, 19.99999999999999645 ) ;
#20249 = CARTESIAN_POINT ( 'NONE',  ( -28.68588794268870856, 339.7448905601784759, 19.99999999999999289 ) ) ;
#20250 =( BOUNDED_CURVE ( )  B_SPLINE_CURVE ( 2, ( #10006, #11747, #8386, #21377, #11533, #9899, #16521, #10117, #19862, #11640, #19640, #13488, #21268, #301, #11853, #88, #13052 ),
 .UNSPECIFIED., .F., .T. ) 
 B_SPLINE_CURVE_WITH_KNOTS ( ( 3, 2, 2, 2, 2, 2, 2, 2, 3 ),
 ( 0.8750000000000002220, 0.8769531250000002220, 0.8789062500000002220, 0.8808593750000002220, 0.8828125000000002220, 0.8847656250000002220, 0.8867187500000002220, 0.8886718750000002220, 0.8906250000000002220 ),
 .UNSPECIFIED. ) 
 CURVE ( )  GEOMETRIC_REPRESENTATION_ITEM ( )  RATIONAL_B_SPLINE_CURVE ( ( 0.9999999999999977796, 0.9807852804032326510, 1.000000000000000000, 0.9807852804032304306, 1.000000000000000000, 0.9807852804032304306, 1.000000000000000000, 0.9807852804032304306, 1.000000000000000000, 0.9807852804032304306, 1.000000000000000000, 0.9807852804032304306, 1.000000000000000000, 0.9807852804032304306, 1.000000000000000000, 0.9807852804032282101, 1.000000000000002220 ) ) 
 REPRESENTATION_ITEM ( '' )  );
#20251 = CARTESIAN_POINT ( 'NONE',  ( -40.53162694259543031, 295.1198905683720000, 11.84573899990672885 ) ) ;
#20252 = CARTESIAN_POINT ( 'NONE',  ( -13.20868407381886023, 379.7448905683720000, 6.410867750099229490 ) ) ;
#20253 = AXIS2_PLACEMENT_3D ( 'NONE', #1656, #11480, #19698 ) ;
#20254 = CARTESIAN_POINT ( 'NONE',  ( -17.35679799567828852, 293.8073905601784759, -16.95518130045146421 ) ) ;
#20255 = EDGE_CURVE ( 'NONE', #10342, #15817, #14332, .T. ) ;
#20256 =( NAMED_UNIT ( * ) SI_UNIT ( $, .STERADIAN. ) SOLID_ANGLE_UNIT ( ) );
#20257 = CARTESIAN_POINT ( 'NONE',  ( -16.84014894278199392, 417.6198905683720000, 11.84573899990672530 ) ) ;
#20258 = CARTESIAN_POINT ( 'NONE',  ( -16.84014894278197971, 261.6198905683720568, -11.84573899990672707 ) ) ;
#20259 = CARTESIAN_POINT ( 'NONE',  ( -25.35362745456399836, 421.0573905683720000, -16.75240474999999307 ) ) ;
#20260 = VECTOR ( 'NONE', #3433, 1000.000000000000000 ) ;
#20261 = CARTESIAN_POINT ( 'NONE',  ( -36.33955658999050797, 360.1198905765656377, -18.47759065022572855 ) ) ;
#20262 = CARTESIAN_POINT ( 'NONE',  ( -47.16347859291443712, 276.6198905601784759, -7.653668647301793193 ) ) ;
#20263 = CARTESIAN_POINT ( 'NONE',  ( -11.93348319268871549, 319.1823905683720568, -3.332260488124732856 ) ) ;
#20264 = CARTESIAN_POINT ( 'NONE',  ( -40.53162694259545162, 474.1198905683720568, -11.84573899990672707 ) ) ;
#20265 = DIRECTION ( 'NONE',  ( -0.000000000000000000, -0.000000000000000000, 1.000000000000000000 ) ) ;
#20266 = EDGE_CURVE ( 'NONE', #8722, #11244, #13270, .T. ) ;
#20267 = CARTESIAN_POINT ( 'NONE',  ( -43.59942232657300565, 200.4092789822994121, -1.616039188923340308 ) ) ;
#20268 = CARTESIAN_POINT ( 'NONE',  ( -11.73070664223724258, 303.1823905601784190, -11.32908994701042538 ) ) ;
#20269 = AXIS2_PLACEMENT_3D ( 'NONE', #6239, #16210, #16003 ) ;
#20270 = CARTESIAN_POINT ( 'NONE',  ( -22.27502019258949062, 382.2448905683720000, -15.47720386886985544 ) ) ;
#20271 = LINE ( 'NONE', #10303, #13379 ) ;
#20272 = CARTESIAN_POINT ( 'NONE',  ( -11.73070664223726745, 531.3073905601785327, 11.32908994701042005 ) ) ;
#20273 = CARTESIAN_POINT ( 'NONE',  ( -42.88789093042843348, 352.9323905683721136, -9.489475012073736337 ) ) ;
#20274 = EDGE_CURVE ( 'NONE', #7137, #15902, #9315, .T. ) ;
#20275 = CIRCLE ( 'NONE', #17180, 20.00000000000000000 ) ;
#20276 = ORIENTED_EDGE ( 'NONE', *, *, #7639, .T. ) ;
#20277 = CARTESIAN_POINT ( 'NONE',  ( -40.53162694259545873, 522.6198905683720568, -11.84573899990672707 ) ) ;
#20278 = ORIENTED_EDGE ( 'NONE', *, *, #17163, .F. ) ;
#20279 = CARTESIAN_POINT ( 'NONE',  ( 1.336753550880579347E-14, 213.9102039777116602, -33.59072564020503648 ) ) ;
#20280 = CARTESIAN_POINT ( 'NONE',  ( -10.20829729246298001, 312.8698905601784759, -7.653668647301794969 ) ) ;
#20281 = LINE ( 'NONE', #9121, #20045 ) ;
#20282 = CARTESIAN_POINT ( 'NONE',  ( -8.685887942688742314, 526.9948905765655809, -2.449293598294705724E-15 ) ) ;
#20283 = CARTESIAN_POINT ( 'NONE',  ( -42.88789093042844769, 474.8073905683720000, 9.489475012073736337 ) ) ;
#20284 = ORIENTED_EDGE ( 'NONE', *, *, #1295, .T. ) ;
#20285 = CARTESIAN_POINT ( 'NONE',  ( -40.53162694259545162, 482.6198905683720000, -11.84573899990672707 ) ) ;
#20286 = CARTESIAN_POINT ( 'NONE',  ( -23.04382792501472821, 45.33667810281676935, -49.27968317789310504 ) ) ;
#20287 = AXIS2_PLACEMENT_3D ( 'NONE', #16174, #11072, #21032 ) ;
#20288 = CARTESIAN_POINT ( 'NONE',  ( -40.01497788969914637, 420.4323905765655809, -16.95518130045146421 ) ) ;
#20289 = CARTESIAN_POINT ( 'NONE',  ( -228.6858879426887654, 610.7448905601785327, 2.449293598294706434E-14 ) ) ;
#20290 = LINE ( 'NONE', #7180, #9218 ) ;
#20291 = PLANE ( 'NONE',  #2894 ) ;
#20292 = CYLINDRICAL_SURFACE ( 'NONE', #20814, 19.99999999999999645 ) ;
#20293 = EDGE_CURVE ( 'NONE', #5413, #16900, #15885, .T. ) ;
#20294 = CARTESIAN_POINT ( 'NONE',  ( 158.8141120573112630, 610.7448905601785327, -10.00000000000000888 ) ) ;
#20295 = CARTESIAN_POINT ( 'NONE',  ( -28.68588794268872277, 434.7448905601784759, -19.99999999999999289 ) ) ;
#20296 = CARTESIAN_POINT ( 'NONE',  ( 0.1061556211655353132, -4.836380039389418073, 4.623144047065560258 ) ) ;
#20297 = CARTESIAN_POINT ( 'NONE',  ( -13.20868407381885135, 290.9948905683720000, -6.410867750099233042 ) ) ;
#20298 = DIRECTION ( 'NONE',  ( 0.000000000000000000, 0.000000000000000000, 1.000000000000000000 ) ) ;
#20299 = CARTESIAN_POINT ( 'NONE',  ( -28.68588794268872633, 442.8698905683720568, -16.75240474999999307 ) ) ;
#20300 = LINE ( 'NONE', #8927, #14754 ) ;
#20301 = CARTESIAN_POINT ( 'NONE',  ( -38.17536295476244845, 273.8073905683720000, -14.20200298773971426 ) ) ;
#20302 = EDGE_CURVE ( 'NONE', #16730, #18163, #5806, .T. ) ;
#20303 = CIRCLE ( 'NONE', #17531, 175.0000000000000284 ) ;
#20304 = ORIENTED_EDGE ( 'NONE', *, *, #12043, .T. ) ;
#20305 = CARTESIAN_POINT ( 'NONE',  ( -11.73070664223727100, 533.1823905601784190, -11.32908994701042538 ) ) ;
#20306 = CARTESIAN_POINT ( 'NONE',  ( -11.93348319268873681, 490.3698905683720568, -2.051577885510841163E-15 ) ) ;
#20307 = ORIENTED_EDGE ( 'NONE', *, *, #9439, .T. ) ;
#20308 = CARTESIAN_POINT ( 'NONE',  ( -11.93348319268873503, 470.0573905683720568, 3.332260488124728415 ) ) ;
#20309 = CARTESIAN_POINT ( 'NONE',  ( -48.68588794268871567, 411.9948905765656377, 0.000000000000000000 ) ) ;
#20310 = CARTESIAN_POINT ( 'NONE',  ( -28.68588794268870146, 251.3698905683720000, -16.75240474999999307 ) ) ;
#20311 = ORIENTED_EDGE ( 'NONE', *, *, #4063, .F. ) ;
#20312 = CARTESIAN_POINT ( 'NONE',  ( -18.68588794268873698, 323.8848358243226357, 20.00000000000000355 ) ) ;
#20313 = CARTESIAN_POINT ( 'NONE',  ( -28.68588794268872633, 474.4948905765656377, 19.99999999999999289 ) ) ;
#20314 = CARTESIAN_POINT ( 'NONE',  ( 69.55160839065807465, 152.8169032537915086, -64.80145223029052204 ) ) ;
#20315 = CARTESIAN_POINT ( 'NONE',  ( -42.88789093042841927, 244.4323905683720284, -9.489475012073734561 ) ) ;
#20316 = CARTESIAN_POINT ( 'NONE',  ( -24.70764059509556532, 419.1823905765655809, -19.99999999999999289 ) ) ;
#20317 = CARTESIAN_POINT ( 'NONE',  ( -8.685887942688706786, 232.5573905601785043, -3.978247347593165895 ) ) ;
#20318 = CARTESIAN_POINT ( 'NONE',  ( -22.27502019258947286, 250.7448905683720000, -15.47720386886985544 ) ) ;
#20319 = CARTESIAN_POINT ( 'NONE',  ( -11.93348319268872082, 360.3698905683720568, -2.051577885510841163E-15 ) ) ;
#20320 = DIRECTION ( 'NONE',  ( 0.000000000000000000, 0.000000000000000000, -1.000000000000000000 ) ) ;
#20321 = CARTESIAN_POINT ( 'NONE',  ( -22.27502019258947996, 396.9948905683720568, 15.47720386886985189 ) ) ;
#20322 = CARTESIAN_POINT ( 'NONE',  ( 158.8141120573112630, 10.52886280891152104, 0.000000000000000000 ) ) ;
#20323 = ADVANCED_FACE ( 'NONE', ( #10885, #7643, #5595 ), #7422, .T. ) ;
#20324 = CARTESIAN_POINT ( 'NONE',  ( -10.20829729246299067, 411.6198905601784759, 7.653668647301790529 ) ) ;
#20325 = VECTOR ( 'NONE', #9735, 1000.000000000000000 ) ;
#20326 = EDGE_CURVE ( 'NONE', #19827, #15737, #18021, .T. ) ;
#20327 = EDGE_LOOP ( 'NONE', ( #8530, #2726, #17903, #443 ) ) ;
#20328 = VERTEX_POINT ( 'NONE', #14798 ) ;
#20329 = ORIENTED_EDGE ( 'NONE', *, *, #733, .F. ) ;
#20330 = CARTESIAN_POINT ( 'NONE',  ( -32.01814843081346851, 523.1823905683720568, -16.75240474999999307 ) ) ;
#20331 = CARTESIAN_POINT ( 'NONE',  ( -45.64106924314017988, 288.1823905601785327, 11.32908994701042715 ) ) ;
#20332 = CARTESIAN_POINT ( 'NONE',  ( -71.26501780185373036, 130.1716627696692683, 1.734723475976807094E-15 ) ) ;
#20333 = VERTEX_POINT ( 'NONE', #16093 ) ;
#20334 = CARTESIAN_POINT ( 'NONE',  ( -32.01814843081344719, 333.1823905683719431, -16.75240474999999307 ) ) ;
#20335 = PRODUCT_RELATED_PRODUCT_CATEGORY ( 'part', '', ( #15993 ) ) ;
#20336 = CARTESIAN_POINT ( 'NONE',  ( -28.68588794268871567, 351.3698905683720568, -16.75240474999999307 ) ) ;
#20337 = CARTESIAN_POINT ( 'NONE',  ( -28.68588794268871212, 356.3698905683720568, 16.75240474999999307 ) ) ;
#20338 = CARTESIAN_POINT ( 'NONE',  ( -48.68588794268870146, 291.9948905765656377, 0.000000000000000000 ) ) ;
#20339 = CARTESIAN_POINT ( 'NONE',  ( -41.83569717483972994, 160.1716627696692683, 25.00000000000000000 ) ) ;
#20340 = CARTESIAN_POINT ( 'NONE',  ( -16.84014894278197971, 270.1198905683720568, -11.84573899990672707 ) ) ;
#20341 = PLANE ( 'NONE',  #15348 ) ;
#20342 = CARTESIAN_POINT ( 'NONE',  ( -22.27502019258948351, 408.4948905683720000, 15.47720386886985189 ) ) ;
#20343 = VECTOR ( 'NONE', #19301, 1000.000000000000227 ) ;
#20344 = CARTESIAN_POINT ( 'NONE',  ( -8.685887942688735208, 548.2448905601784190, 2.449293598294706513E-15 ) ) ;
#20345 = CARTESIAN_POINT ( 'NONE',  ( 105.7989814974898479, 152.5259582928263740, 40.00000000000000000 ) ) ;
#20346 = CARTESIAN_POINT ( 'NONE',  ( -40.01497788969913927, 408.8073905601784759, 16.95518130045146776 ) ) ;
#20347 = CARTESIAN_POINT ( 'NONE',  ( -38.17536295476245556, 333.8073905683720000, -14.20200298773971426 ) ) ;
#20348 = CARTESIAN_POINT ( 'NONE',  ( -44.16309181155857999, 464.4948905683720000, 6.410867750099241924 ) ) ;
#20349 = EDGE_LOOP ( 'NONE', ( #3440, #17453, #7142, #6142, #15028, #15659 ) ) ;
#20350 = CARTESIAN_POINT ( 'NONE',  ( -40.01497788969915348, 465.6823905601785327, -16.95518130045146421 ) ) ;
#20351 = CARTESIAN_POINT ( 'NONE',  ( -38.17536295476244135, 285.4323905683720568, 14.20200298773971781 ) ) ;
#20352 = ORIENTED_EDGE ( 'NONE', *, *, #14073, .F. ) ;
#20353 = ORIENTED_EDGE ( 'NONE', *, *, #1303, .T. ) ;
#20354 = DIRECTION ( 'NONE',  ( 1.191790137725560488E-16, -1.000000000000000000, -0.000000000000000000 ) ) ;
#20355 = CARTESIAN_POINT ( 'NONE',  ( -21.03221929538691981, 344.1198905601784759, -18.47759065022572855 ) ) ;
#20356 = CARTESIAN_POINT ( 'NONE',  ( -35.09675569278794427, 295.7448905683720568, 15.47720386886985366 ) ) ;
#20357 = VECTOR ( 'NONE', #17857, 1000.000000000000000 ) ;
#20358 = CARTESIAN_POINT ( 'NONE',  ( -42.88789093042843348, 374.4323905683720000, -9.489475012073734561 ) ) ;
#20359 = CARTESIAN_POINT ( 'NONE',  ( -28.68588794268869435, 229.7448905601785043, 19.99999999999999289 ) ) ;
#20360 = CARTESIAN_POINT ( 'NONE',  ( -42.82802356641968089, 530.7448905765656946, -14.14213562373094746 ) ) ;
#20361 = CARTESIAN_POINT ( 'NONE',  ( -13.20868407381886556, 399.4948905683720000, -6.410867750099233042 ) ) ;
#20362 = CARTESIAN_POINT ( 'NONE',  ( -25.35362745456396638, 258.1823905683720000, 16.75240474999998952 ) ) ;
#20363 = CARTESIAN_POINT ( 'NONE',  ( -11.93348319268872970, 428.8698905683720568, -2.051577885510841163E-15 ) ) ;
#20364 = CONTEXT_DEPENDENT_SHAPE_REPRESENTATION ( #19952, #17352 ) ;
#20365 = CARTESIAN_POINT ( 'NONE',  ( -32.66413529028187668, 339.8073905765656377, -19.99999999999999289 ) ) ;
#20366 = DIRECTION ( 'NONE',  ( -0.000000000000000000, 1.000000000000000000, -0.000000000000000000 ) ) ;
#20367 = CARTESIAN_POINT ( 'NONE',  ( -40.53162694259543031, 325.1198905683720568, 11.84573899990672885 ) ) ;
#20368 = CARTESIAN_POINT ( 'NONE',  ( -28.68588794268872988, 472.8698905683720568, -16.75240474999999307 ) ) ;
#20369 = CARTESIAN_POINT ( 'NONE',  ( -17.35679799567829917, 435.4323905765656377, 16.95518130045146421 ) ) ;
#20370 = CARTESIAN_POINT ( 'NONE',  ( -71.26501780185373036, 130.1716627696692683, 25.00000000000000355 ) ) ;
#20371 = CYLINDRICAL_SURFACE ( 'NONE', #14737, 19.99999999999999645 ) ;
#20372 = VECTOR ( 'NONE', #2939, 1000.000000000000000 ) ;
#20373 = CARTESIAN_POINT ( 'NONE',  ( -14.48388495494899963, 379.4323905683721136, 9.489475012073732785 ) ) ;
#20374 = CARTESIAN_POINT ( 'NONE',  ( -28.05147542941067229, 46.81912526956768517, -121.8134868412888494 ) ) ;
#20375 = EDGE_CURVE ( 'NONE', #8258, #3061, #9408, .T. ) ;
#20376 =( BOUNDED_CURVE ( )  B_SPLINE_CURVE ( 2, ( #17368, #10432, #15861, #3951, #7611, #20716, #3845, #20606, #7293, #20395, #17054, #8815, #13918, #2339, #15432, #2655, #5781 ),
 .UNSPECIFIED., .F., .T. ) 
 B_SPLINE_CURVE_WITH_KNOTS ( ( 3, 2, 2, 2, 2, 2, 2, 2, 3 ),
 ( 0.1406250000000001388, 0.1425781250000001388, 0.1445312500000001388, 0.1464843750000001388, 0.1484375000000001388, 0.1503906250000001388, 0.1523437500000001388, 0.1542968750000001388, 0.1562500000000001388 ),
 .UNSPECIFIED. ) 
 CURVE ( )  GEOMETRIC_REPRESENTATION_ITEM ( )  RATIONAL_B_SPLINE_CURVE ( ( 0.9999999999999986677, 0.9807852804032317628, 1.000000000000000000, 0.9807852804032304306, 1.000000000000000000, 0.9807852804032304306, 1.000000000000000000, 0.9807852804032304306, 1.000000000000000000, 0.9807852804032304306, 1.000000000000000000, 0.9807852804032304306, 1.000000000000000000, 0.9807852804032304306, 1.000000000000000000, 0.9807852804032290983, 1.000000000000001332 ) ) 
 REPRESENTATION_ITEM ( '' )  );
#20377 = CARTESIAN_POINT ( 'NONE',  ( -36.33955658999053639, 519.1198905601785327, 18.47759065022572500 ) ) ;
#20378 = CARTESIAN_POINT ( 'NONE',  ( -45.43829269268870519, 353.5573905683721136, -3.332260488124726194 ) ) ;
#20379 = ORIENTED_EDGE ( 'NONE', *, *, #388, .T. ) ;
#20380 = CARTESIAN_POINT ( 'NONE',  ( -19.19641293061499709, 497.3073905683720568, 14.20200298773971426 ) ) ;
#20381 = VERTEX_POINT ( 'NONE', #11315 ) ;
#20382 = CARTESIAN_POINT ( 'NONE',  ( -32.66413529028187668, 349.4323905601785327, 19.99999999999999289 ) ) ;
#20383 = DIRECTION ( 'NONE',  ( -0.000000000000000000, -0.000000000000000000, -1.000000000000000000 ) ) ;
#20384 = CARTESIAN_POINT ( 'NONE',  ( -123.2946569474810161, 30.52886280891152282, 20.57735571454641388 ) ) ;
#20385 = CARTESIAN_POINT ( 'NONE',  ( -10.76731745429010090, 56.85652257517428865, 46.25122601329427141 ) ) ;
#20386 = CARTESIAN_POINT ( 'NONE',  ( 30.42502041961814996, 170.1716627696692683, 20.00000000000000355 ) ) ;
#20387 = CARTESIAN_POINT ( 'NONE',  ( -28.68588794268872988, 461.3698905683720000, -16.75240474999999307 ) ) ;
#20388 = ORIENTED_EDGE ( 'NONE', *, *, #5344, .T. ) ;
#20389 = CARTESIAN_POINT ( 'NONE',  ( -44.16309181155857999, 494.4948905683720568, 6.410867750099241924 ) ) ;
#20390 = CARTESIAN_POINT ( 'NONE',  ( -8.685887942688708563, 246.9948905765656093, -2.449293598294705724E-15 ) ) ;
#20391 = CARTESIAN_POINT ( 'NONE',  ( -47.16347859291445133, 432.6198905765656377, 7.653668647301805628 ) ) ;
#20392 = CARTESIAN_POINT ( 'NONE',  ( -8.685887942688735208, 476.9948905765656377, -2.449293598294705724E-15 ) ) ;
#20393 = FACE_OUTER_BOUND ( 'NONE', #6696, .T. ) ;
#20394 = LINE ( 'NONE', #17053, #17403 ) ;
#20395 = CARTESIAN_POINT ( 'NONE',  ( -32.66413529028188378, 484.1823905765656946, 19.99999999999999289 ) ) ;
#20396 = EDGE_CURVE ( 'NONE', #19138, #9067, #18984, .T. ) ;
#20397 = AXIS2_PLACEMENT_3D ( 'NONE', #10554, #5691, #15665 ) ;
#20398 = LINE ( 'NONE', #12177, #11643 ) ;
#20399 = CARTESIAN_POINT ( 'NONE',  ( -24.70764059509556532, 434.4323905601785327, -19.99999999999999289 ) ) ;
#20400 = CARTESIAN_POINT ( 'NONE',  ( 0.000000000000000000, -5.629165124598843661, 3.250000000000012434 ) ) ;
#20401 = CARTESIAN_POINT ( 'NONE',  ( -14.48388495494898720, 279.4323905683720568, 9.489475012073732785 ) ) ;
#20402 = CARTESIAN_POINT ( 'NONE',  ( -28.68588794268869790, 249.7448905601784475, 19.99999999999999289 ) ) ;
#20403 = LINE ( 'NONE', #12395, #15102 ) ;
#20404 = CARTESIAN_POINT ( 'NONE',  ( -45.43829269268872650, 455.3698905683720000, 0.000000000000000000 ) ) ;
#20405 = CARTESIAN_POINT ( 'NONE',  ( -47.16347859291445133, 401.3698905765656377, -7.653668647301793193 ) ) ;
#20406 = CARTESIAN_POINT ( 'NONE',  ( -44.16309181155855157, 265.9948905683720000, 6.410867750099241924 ) ) ;
#20407 = EDGE_LOOP ( 'NONE', ( #6856, #8800, #10112, #11140 ) ) ;
#20408 = CIRCLE ( 'NONE', #12062, 10.00000000000000178 ) ;
#20409 = CARTESIAN_POINT ( 'NONE',  ( 6.416697501590670427, 172.9933428177121471, 50.00000000000000000 ) ) ;
#20410 = CARTESIAN_POINT ( 'NONE',  ( -45.43829269268872650, 475.0573905683720000, -3.332260488124726638 ) ) ;
#20411 = EDGE_CURVE ( 'NONE', #2296, #1002, #19753, .T. ) ;
#20412 = AXIS2_PLACEMENT_3D ( 'NONE', #7404, #519, #15546 ) ;
#20413 = AXIS2_PLACEMENT_3D ( 'NONE', #17836, #14188, #20780 ) ;
#20414 = EDGE_LOOP ( 'NONE', ( #3039, #9466, #4097, #15321 ) ) ;
#20415 = CARTESIAN_POINT ( 'NONE',  ( -48.68588794268871567, 401.9948905765656377, 0.000000000000000000 ) ) ;
#20416 = CARTESIAN_POINT ( 'NONE',  ( -45.43829269268869808, 253.8698905683720000, 0.000000000000000000 ) ) ;
#20417 = ORIENTED_EDGE ( 'NONE', *, *, #6166, .T. ) ;
#20418 = FACE_OUTER_BOUND ( 'NONE', #10467, .T. ) ;
#20419 = CARTESIAN_POINT ( 'NONE',  ( -48.68588794268872277, 481.6823905765656377, -3.978247347593158345 ) ) ;
#20420 = DIRECTION ( 'NONE',  ( -0.000000000000000000, 1.000000000000000000, -0.000000000000000000 ) ) ;
#20421 = CARTESIAN_POINT ( 'NONE',  ( -11.93348319268870661, 240.6823905683720284, -3.332260488124732856 ) ) ;
#20422 = EDGE_CURVE ( 'NONE', #8699, #19163, #14478, .T. ) ;
#20423 = CARTESIAN_POINT ( 'NONE',  ( -42.82802356641965957, 365.9948905601784759, -14.14213562373094746 ) ) ;
#20424 = CARTESIAN_POINT ( 'NONE',  ( -28.68588794268872988, 517.8698905683720568, 16.75240474999999307 ) ) ;
#20425 = CARTESIAN_POINT ( 'NONE',  ( -47.16347859291444422, 372.6198905765655809, 7.653668647301805628 ) ) ;
#20426 = CARTESIAN_POINT ( 'NONE',  ( -22.27502019258946220, 246.9948905683720284, 15.47720386886985189 ) ) ;
#20427 = CARTESIAN_POINT ( 'NONE',  ( -40.53162694259543741, 334.1198905683720568, -11.84573899990672707 ) ) ;
#20428 = CARTESIAN_POINT ( 'NONE',  ( -24.70764059509554755, 320.0573905601784759, 19.99999999999998934 ) ) ;
#20429 = VECTOR ( 'NONE', #3464, 1000.000000000000000 ) ;
#20430 = CARTESIAN_POINT ( 'NONE',  ( -35.09675569278795848, 405.7448905683720568, 15.47720386886985366 ) ) ;
#20431 = CARTESIAN_POINT ( 'NONE',  ( 2.416697501590669095, 217.7548513357008630, 45.00000000000000000 ) ) ;
#20432 = CARTESIAN_POINT ( 'NONE',  ( -28.68588794268871922, 404.7448905601784759, -19.99999999999999289 ) ) ;
#20433 = ORIENTED_EDGE ( 'NONE', *, *, #16475, .F. ) ;
#20434 = DIRECTION ( 'NONE',  ( -1.000000000000000000, 0.000000000000000000, 0.000000000000000000 ) ) ;
#20435 = ORIENTED_EDGE ( 'NONE', *, *, #14622, .F. ) ;
#20436 = ORIENTED_EDGE ( 'NONE', *, *, #1969, .F. ) ;
#20437 = CARTESIAN_POINT ( 'NONE',  ( -42.88789093042844769, 504.4323905683721136, -9.489475012073736337 ) ) ;
#20438 = CARTESIAN_POINT ( 'NONE',  ( -21.03221929538690205, 290.3698905601784759, 18.47759065022572500 ) ) ;
#20439 = CARTESIAN_POINT ( 'NONE',  ( -43.04742826731176564, 207.6584868706943041, -4.333760535973599559 ) ) ;
#20440 = ORIENTED_EDGE ( 'NONE', *, *, #12390, .T. ) ;
#20441 = CARTESIAN_POINT ( 'NONE',  ( -19.19641293061497933, 331.9323905683720000, -14.20200298773971603 ) ) ;
#20442 = AXIS2_PLACEMENT_3D ( 'NONE', #1722, #1610, #13294 ) ;
#20443 = VERTEX_POINT ( 'NONE', #14693 ) ;
#20444 = CARTESIAN_POINT ( 'NONE',  ( -45.43829269268870519, 353.5573905683721136, -3.332260488124726194 ) ) ;
#20445 = CARTESIAN_POINT ( 'NONE',  ( -14.48388495494899786, 349.8073905683720000, -9.489475012073734561 ) ) ;
#20446 = CARTESIAN_POINT ( 'NONE',  ( -8.685887942688713892, 286.6823905765656377, 3.978247347593161010 ) ) ;
#20447 = CARTESIAN_POINT ( 'NONE',  ( -48.68588794268865882, 501.6823905765654672, -3.978247347593317773 ) ) ;
#20448 = CARTESIAN_POINT ( 'NONE',  ( -35.09675569278793006, 251.9948905683720568, -15.47720386886985544 ) ) ;
#20449 = DIRECTION ( 'NONE',  ( 0.000000000000000000, -0.000000000000000000, 1.000000000000000000 ) ) ;
#20450 = ADVANCED_FACE ( 'NONE', ( #19541, #2792, #11420 ), #9587, .F. ) ;
#20451 = CARTESIAN_POINT ( 'NONE',  ( -16.84014894278199748, 411.6198905683720568, -11.84573899990672707 ) ) ;
#20452 = CARTESIAN_POINT ( 'NONE',  ( 158.8141120573112630, 400.5398297725603243, -9.999999999999980460 ) ) ;
#20453 = CARTESIAN_POINT ( 'NONE',  ( -45.64106924314017988, 356.3073905601785896, -11.32908994701042538 ) ) ;
#20454 = UNCERTAINTY_MEASURE_WITH_UNIT (LENGTH_MEASURE( 1.000000000000000082E-05 ), #5224, 'distance_accuracy_value', 'NONE');
#20455 = CARTESIAN_POINT ( 'NONE',  ( -42.82802356641966668, 408.4948905601784759, 14.14213562373094923 ) ) ;
#20456 = CARTESIAN_POINT ( 'NONE',  ( -11.93348319268871549, 320.3698905683720568, -2.051577885510841163E-15 ) ) ;
#20457 = CARTESIAN_POINT ( 'NONE',  ( -42.88789093042844769, 454.8073905683720000, 9.489475012073736337 ) ) ;
#20458 = ORIENTED_EDGE ( 'NONE', *, *, #21380, .F. ) ;
#20459 = AXIS2_PLACEMENT_3D ( 'NONE', #17998, #15967, #3081 ) ;
#20460 = CARTESIAN_POINT ( 'NONE',  ( -45.64106924314020119, 476.3073905601785327, -11.32908994701042715 ) ) ;
#20461 = CARTESIAN_POINT ( 'NONE',  ( -14.48388495494899075, 279.8073905683720000, -9.489475012073736337 ) ) ;
#20462 = EDGE_CURVE ( 'NONE', #683, #16932, #3215, .T. ) ;
#20463 = ORIENTED_EDGE ( 'NONE', *, *, #3021, .T. ) ;
#20464 = CARTESIAN_POINT ( 'NONE',  ( -49.57497958038186425, 230.5765313837437418, 49.99999999999999289 ) ) ;
#20465 = CARTESIAN_POINT ( 'NONE',  ( -22.27502019258949773, 452.2448905683720000, -15.47720386886985544 ) ) ;
#20466 = ORIENTED_EDGE ( 'NONE', *, *, #730, .T. ) ;
#20467 = LINE ( 'NONE', #5955, #7321 ) ;
#20468 = ADVANCED_FACE ( 'NONE', ( #9794, #17910, #4618 ), #14376, .F. ) ;
#20469 = CARTESIAN_POINT ( 'NONE',  ( -25.35362745456397349, 306.6823905683720000, 16.75240474999998952 ) ) ;
#20470 = EDGE_CURVE ( 'NONE', #2640, #8642, #14583, .T. ) ;
#20471 = CARTESIAN_POINT ( 'NONE',  ( -19.19641293061498288, 378.8073905683721136, 14.20200298773971426 ) ) ;
#20472 = CARTESIAN_POINT ( 'NONE',  ( -8.685887942688795604, 231.9323905601784759, 3.978247347593374172 ) ) ;
#20473 = CARTESIAN_POINT ( 'NONE',  ( -21.03221929538692692, 515.1198905765656946, 18.47759065022572500 ) ) ;
#20474 = CARTESIAN_POINT ( 'NONE',  ( -11.93348319268872615, 399.1823905683720568, -3.332260488124732856 ) ) ;
#20475 = CARTESIAN_POINT ( 'NONE',  ( -22.27502019258946220, 248.4948905683720284, 15.47720386886985189 ) ) ;
#20476 = CARTESIAN_POINT ( 'NONE',  ( -11.93348319268872970, 428.5573905683720568, 3.332260488124728859 ) ) ;
#20477 = CARTESIAN_POINT ( 'NONE',  ( -14.54375231895776466, 335.7448905765655809, 14.14213562373094568 ) ) ;
#20478 = CARTESIAN_POINT ( 'NONE',  ( -43.68588794268869435, 188.9102039777116602, 0.000000000000000000 ) ) ;
#20479 = CARTESIAN_POINT ( 'NONE',  ( -19.19641293061497223, 307.3073905683720000, 14.20200298773971426 ) ) ;
#20480 = CARTESIAN_POINT ( 'NONE',  ( -40.53162694259545162, 476.6198905683720000, 11.84573899990672885 ) ) ;
#20481 = EDGE_CURVE ( 'NONE', #12774, #1814, #12876, .T. ) ;
#20482 = DIRECTION ( 'NONE',  ( 0.9999562017632421806, 0.000000000000000000, 0.009359196291876339252 ) ) ;
#20483 = CARTESIAN_POINT ( 'NONE',  ( -43.68588794268868725, 200.1437886375728397, -0.3328713742805504139 ) ) ;
#20484 = DIRECTION ( 'NONE',  ( -0.000000000000000000, -0.000000000000000000, 1.000000000000000000 ) ) ;
#20485 = CARTESIAN_POINT ( 'NONE',  ( -25.35362745456399480, 382.5573905683720568, -16.75240474999999307 ) ) ;
#20486 = CARTESIAN_POINT ( 'NONE',  ( -43.68588794268869435, 210.1437886375728965, -2.161864096862809871E-19 ) ) ;
#20487 = AXIS2_PLACEMENT_3D ( 'NONE', #14477, #17809, #16201 ) ;
#20488 = CARTESIAN_POINT ( 'NONE',  ( -32.66413529028189799, 525.0573905601784190, -19.99999999999999289 ) ) ;
#20489 = CARTESIAN_POINT ( 'NONE',  ( -22.27502019258948351, 340.7448905683720568, -15.47720386886985544 ) ) ;
#20490 = VERTEX_POINT ( 'NONE', #6128 ) ;
#20491 = CARTESIAN_POINT ( 'NONE',  ( -42.88789093042845479, 504.8073905683720568, 9.489475012073736337 ) ) ;
#20492 = ORIENTED_EDGE ( 'NONE', *, *, #13291, .T. ) ;
#20493 = CARTESIAN_POINT ( 'NONE',  ( -32.66413529028187668, 355.0573905601785327, -19.99999999999999289 ) ) ;
#20494 = CARTESIAN_POINT ( 'NONE',  ( -11.73070664223724968, 377.9323905765656946, -11.32908994701042538 ) ) ;
#20495 = PLANE ( 'NONE',  #15344 ) ;
#20496 = DIRECTION ( 'NONE',  ( 0.000000000000000000, 1.000000000000000000, 0.000000000000000000 ) ) ;
#20497 = DIRECTION ( 'NONE',  ( -1.191790137725560488E-16, 1.000000000000000000, -0.000000000000000000 ) ) ;
#20498 = CARTESIAN_POINT ( 'NONE',  ( -16.84014894278200103, 467.6198905683720000, 11.84573899990672530 ) ) ;
#20499 = ORIENTED_EDGE ( 'NONE', *, *, #1392, .F. ) ;
#20500 = CARTESIAN_POINT ( 'NONE',  ( -11.93348319268873503, 478.8698905683720568, -2.051577885510841163E-15 ) ) ;
#20501 = CARTESIAN_POINT ( 'NONE',  ( -36.33955658999050087, 243.8698905765656093, 18.47759065022572500 ) ) ;
#20502 = AXIS2_PLACEMENT_3D ( 'NONE', #1088, #11328, #9598 ) ;
#20503 = CARTESIAN_POINT ( 'NONE',  ( -28.68588794268871922, 399.4948905765656377, -19.99999999999999289 ) ) ;
#20504 = DIRECTION ( 'NONE',  ( -1.000000000000000000, -0.000000000000000000, -0.000000000000000000 ) ) ;
#20505 = CARTESIAN_POINT ( 'NONE',  ( -47.16347859291443712, 297.8698905601784759, 7.653668647301805628 ) ) ;
#20506 = CARTESIAN_POINT ( 'NONE',  ( -11.73070664223726389, 483.1823905601784190, -11.32908994701042538 ) ) ;
#20507 = CARTESIAN_POINT ( 'NONE',  ( -28.68588794268872633, 378.8848358243226357, 0.000000000000000000 ) ) ;
#20508 = CIRCLE ( 'NONE', #11164, 6.500000000000000888 ) ;
#20509 = CARTESIAN_POINT ( 'NONE',  ( -28.68588794268874054, 573.2448905601785327, 0.000000000000000000 ) ) ;
#20510 = DIRECTION ( 'NONE',  ( 0.7723044064191042501, 0.000000000000000000, -0.6352526299242178265 ) ) ;
#20511 =( BOUNDED_CURVE ( )  B_SPLINE_CURVE ( 2, ( #17797, #2987, #16080, #16402, #6422, #13038, #1688, #21046, #8150, #19628, #19312, #1579, #12830, #6112, #4807, #14678, #8259 ),
 .UNSPECIFIED., .F., .T. ) 
 B_SPLINE_CURVE_WITH_KNOTS ( ( 3, 2, 2, 2, 2, 2, 2, 2, 3 ),
 ( 0.3281250000000001110, 0.3300781250000001110, 0.3320312500000001110, 0.3339843750000001110, 0.3359375000000001110, 0.3378906250000001110, 0.3398437500000001110, 0.3417968750000001110, 0.3437500000000001110 ),
 .UNSPECIFIED. ) 
 CURVE ( )  GEOMETRIC_REPRESENTATION_ITEM ( )  RATIONAL_B_SPLINE_CURVE ( ( 0.9999999999999988898, 0.9807852804032315408, 1.000000000000000000, 0.9807852804032304306, 1.000000000000000000, 0.9807852804032304306, 1.000000000000000000, 0.9807852804032304306, 1.000000000000000000, 0.9807852804032304306, 1.000000000000000000, 0.9807852804032304306, 1.000000000000000000, 0.9807852804032304306, 1.000000000000000000, 0.9807852804032293204, 1.000000000000001110 ) ) 
 REPRESENTATION_ITEM ( '' )  );
#20512 = CARTESIAN_POINT ( 'NONE',  ( -42.88789093042842637, 276.3073905683720568, 9.489475012073736337 ) ) ;
#20513 = CARTESIAN_POINT ( 'NONE',  ( -42.82802356641964536, 255.9948905601784759, -14.14213562373094746 ) ) ;
#20514 = CARTESIAN_POINT ( 'NONE',  ( -64.27068722059112815, 600.7448905601785327, -35.12437985717895828 ) ) ;
#20515 = CARTESIAN_POINT ( 'NONE',  ( -35.09675569278795138, 443.4948905683720568, -15.47720386886985544 ) ) ;
#20516 = CARTESIAN_POINT ( 'NONE',  ( 4.700000000000000178, 7.505553499465139389, 0.000000000000000000 ) ) ;
#20517 = CARTESIAN_POINT ( 'NONE',  ( -13.20868407381884779, 260.9948905683720568, -6.410867750099233042 ) ) ;
#20518 = VECTOR ( 'NONE', #7710, 999.9999999999998863 ) ;
#20519 = ORIENTED_EDGE ( 'NONE', *, *, #4926, .T. ) ;
#20520 = CARTESIAN_POINT ( 'NONE',  ( -28.68588794268874054, 573.2448905601785327, 0.000000000000000000 ) ) ;
#20521 = ORIENTED_EDGE ( 'NONE', *, *, #18647, .T. ) ;
#20522 = CARTESIAN_POINT ( 'NONE',  ( -35.09675569278795848, 483.4948905683720000, -15.47720386886985544 ) ) ;
#20523 = VECTOR ( 'NONE', #13168, 1000.000000000000000 ) ;
#20524 = EDGE_CURVE ( 'NONE', #17823, #4779, #1490, .T. ) ;
#20525 = ORIENTED_EDGE ( 'NONE', *, *, #13079, .F. ) ;
#20526 = CARTESIAN_POINT ( 'NONE',  ( 4.700000000000000178, -7.505553499465150047, 0.000000000000000000 ) ) ;
#20527 = CARTESIAN_POINT ( 'NONE',  ( -44.16309181155855867, 233.2448905683720000, -6.410867750099231266 ) ) ;
#20528 = VERTEX_POINT ( 'NONE', #11749 ) ;
#20529 = DIRECTION ( 'NONE',  ( -9.855701800883827197E-17, 1.000000000000000000, 9.855701800883827197E-17 ) ) ;
#20530 = CARTESIAN_POINT ( 'NONE',  ( -28.68588794268872988, 459.4948905765656377, -19.99999999999999289 ) ) ;
#20531 = LINE ( 'NONE', #15671, #10993 ) ;
#20532 = CARTESIAN_POINT ( 'NONE',  ( -25.35362745456397704, 232.5573905683720568, -16.75240474999999307 ) ) ;
#20533 = CARTESIAN_POINT ( 'NONE',  ( -38.17536295476247687, 513.8073905683720568, -14.20200298773971426 ) ) ;
#20534 = CARTESIAN_POINT ( 'NONE',  ( 60.03793209889851568, 30.52886280891152282, 126.1729372809868863 ) ) ;
#20535 = CARTESIAN_POINT ( 'NONE',  ( -35.09675569278793716, 245.7448905683720000, 15.47720386886985366 ) ) ;
#20536 = AXIS2_PLACEMENT_3D ( 'NONE', #3492, #10077, #6938 ) ;
#20537 = CARTESIAN_POINT ( 'NONE',  ( -42.88789093042843348, 344.4323905683720000, -9.489475012073736337 ) ) ;
#20538 = ADVANCED_FACE ( 'NONE', ( #9901 ), #20187, .T. ) ;
#20539 = CARTESIAN_POINT ( 'NONE',  ( -49.57497958038185715, 160.1716627696692683, 60.00000000000000000 ) ) ;
#20540 = CARTESIAN_POINT ( 'NONE',  ( -48.68588794268870146, 301.9948905765655809, 0.000000000000000000 ) ) ;
#20541 = CARTESIAN_POINT ( 'NONE',  ( -42.88789093042843348, 384.8073905683720000, 9.489475012073736337 ) ) ;
#20542 = CARTESIAN_POINT ( 'NONE',  ( -24.70764059509555466, 380.0573905601785327, 19.99999999999998934 ) ) ;
#20543 = ADVANCED_FACE ( 'NONE', ( #5041 ), #11641, .F. ) ;
#20544 = ORIENTED_EDGE ( 'NONE', *, *, #5382, .T. ) ;
#20545 = CARTESIAN_POINT ( 'NONE',  ( -10.20829729246298356, 347.6198905765656377, -7.653668647301794969 ) ) ;
#20546 = ORIENTED_EDGE ( 'NONE', *, *, #16856, .F. ) ;
#20547 = ORIENTED_EDGE ( 'NONE', *, *, #15576, .F. ) ;
#20548 = CARTESIAN_POINT ( 'NONE',  ( -40.53162694259545873, 516.6198905683720568, 11.84573899990672885 ) ) ;
#20549 = CARTESIAN_POINT ( 'NONE',  ( -47.16347859291443712, 292.6198905765656377, 7.653668647301805628 ) ) ;
#20550 = ORIENTED_EDGE ( 'NONE', *, *, #17488, .T. ) ;
#20551 = CARTESIAN_POINT ( 'NONE',  ( -16.84014894278198327, 301.6198905683720000, -11.84573899990672707 ) ) ;
#20552 = ORIENTED_EDGE ( 'NONE', *, *, #19396, .F. ) ;
#20553 = CARTESIAN_POINT ( 'NONE',  ( -38.17536295476245556, 352.3073905683720000, -14.20200298773971426 ) ) ;
#20554 = CARTESIAN_POINT ( 'NONE',  ( -16.84014894278198682, 347.6198905683720000, 11.84573899990672530 ) ) ;
#20555 = CARTESIAN_POINT ( 'NONE',  ( -8.685887942688713892, 286.9948905765656377, -2.449293598294705724E-15 ) ) ;
#20556 = FACE_OUTER_BOUND ( 'NONE', #11889, .T. ) ;
#20557 = CARTESIAN_POINT ( 'NONE',  ( -14.48388495494898542, 249.8073905683720284, -9.489475012073734561 ) ) ;
#20558 = CARTESIAN_POINT ( 'NONE',  ( -43.64324723180578047, 200.2731091681331179, 1.141620385913097779 ) ) ;
#20559 = CARTESIAN_POINT ( 'NONE',  ( -25.35362745456399480, 392.5573905683720000, -16.75240474999999307 ) ) ;
#20560 = CARTESIAN_POINT ( 'NONE',  ( 51.98438129372387806, 56.85652257517428865, -117.7249735956185219 ) ) ;
#20561 = CARTESIAN_POINT ( 'NONE',  ( -32.66413529028189089, 509.8073905765655240, -19.99999999999999289 ) ) ;
#20562 = CIRCLE ( 'NONE', #15696, 43.46661168214937732 ) ;
#20563 = CARTESIAN_POINT ( 'NONE',  ( -25.35362745456400191, 461.0573905683721136, -16.75240474999999307 ) ) ;
#20564 = EDGE_LOOP ( 'NONE', ( #8513, #4365, #6111, #15525 ) ) ;
#20565 = CARTESIAN_POINT ( 'NONE',  ( -36.33955658999052218, 449.1198905601784759, 18.47759065022572500 ) ) ;
#20566 = CARTESIAN_POINT ( 'NONE',  ( -11.93348319268871194, 278.5573905683720000, 3.332260488124728415 ) ) ;
#20567 = ORIENTED_EDGE ( 'NONE', *, *, #3150, .F. ) ;
#20568 = ORIENTED_EDGE ( 'NONE', *, *, #18598, .T. ) ;
#20569 = ORIENTED_EDGE ( 'NONE', *, *, #13811, .F. ) ;
#20570 = CARTESIAN_POINT ( 'NONE',  ( -28.68588794268869435, 188.9102039777116602, 0.000000000000000000 ) ) ;
#20571 = CARTESIAN_POINT ( 'NONE',  ( -42.82802356641965957, 348.4948905601785327, 14.14213562373094923 ) ) ;
#20572 = CARTESIAN_POINT ( 'NONE',  ( -11.93348319268871371, 298.8698905683720000, -2.051577885510841163E-15 ) ) ;
#20573 = CARTESIAN_POINT ( 'NONE',  ( -19.19641293061498288, 371.9323905683720568, -14.20200298773971603 ) ) ;
#20574 = CARTESIAN_POINT ( 'NONE',  ( -18.81370552131602736, 600.7448905601785327, -6.112943483001347822 ) ) ;
#20575 = CARTESIAN_POINT ( 'NONE',  ( -36.33955658999053639, 513.8698905765655809, 18.47759065022572500 ) ) ;
#20576 = CARTESIAN_POINT ( 'NONE',  ( -25.35362745456398770, 406.6823905683720000, 16.75240474999998952 ) ) ;
#20577 = CARTESIAN_POINT ( 'NONE',  ( -14.48388495494898365, 249.4323905683720000, 9.489475012073732785 ) ) ;
#20578 = CARTESIAN_POINT ( 'NONE',  ( -19.19641293061498999, 410.4323905683720568, -14.20200298773971603 ) ) ;
#20579 = CARTESIAN_POINT ( 'NONE',  ( -42.82802356641965957, 353.2448905765656377, 14.14213562373094923 ) ) ;
#20580 = CARTESIAN_POINT ( 'NONE',  ( 5.674999999999999822, -3.752776749732561257, 6.500000000000000000 ) ) ;
#20581 = CARTESIAN_POINT ( 'NONE',  ( -22.27502019258947996, 310.7448905683720000, -15.47720386886985544 ) ) ;
#20582 = CARTESIAN_POINT ( 'NONE',  ( -32.01814843081346140, 457.5573905683720000, 16.75240474999999307 ) ) ;
#20583 = CARTESIAN_POINT ( 'NONE',  ( -17.35679799567830628, 515.4323905765656946, 16.95518130045146421 ) ) ;
#20584 = DIRECTION ( 'NONE',  ( -0.8090169943749474513, 0.000000000000000000, -0.5877852522924730261 ) ) ;
#20585 = CARTESIAN_POINT ( 'NONE',  ( -73.08746600497821078, 600.7448905601785327, 22.98912494155475628 ) ) ;
#20586 = EDGE_CURVE ( 'NONE', #74, #7286, #16947, .T. ) ;
#20587 = CARTESIAN_POINT ( 'NONE',  ( -35.09675569278794427, 363.4948905683720568, -15.47720386886985544 ) ) ;
#20588 = FACE_OUTER_BOUND ( 'NONE', #7779, .T. ) ;
#20589 = CARTESIAN_POINT ( 'NONE',  ( -10.20829729246300666, 531.6198905601785327, 7.653668647301790529 ) ) ;
#20590 = CARTESIAN_POINT ( 'NONE',  ( -32.01814843081344719, 341.6823905683720000, -16.75240474999999307 ) ) ;
#20591 = ORIENTED_EDGE ( 'NONE', *, *, #4309, .F. ) ;
#20592 = CARTESIAN_POINT ( 'NONE',  ( -32.01814843081346140, 501.6823905683720568, -16.75240474999999307 ) ) ;
#20593 = ORIENTED_EDGE ( 'NONE', *, *, #19055, .T. ) ;
#20594 = CARTESIAN_POINT ( 'NONE',  ( -14.54375231895777176, 378.2448905765656377, -14.14213562373094746 ) ) ;
#20595 = LINE ( 'NONE', #823, #19471 ) ;
#20596 = EDGE_CURVE ( 'NONE', #21094, #5930, #20832, .T. ) ;
#20597 = DIRECTION ( 'NONE',  ( -0.000000000000000000, -1.000000000000000000, -0.000000000000000000 ) ) ;
#20598 = CARTESIAN_POINT ( 'NONE',  ( -25.35362745456400546, 471.0573905683720568, -16.75240474999999307 ) ) ;
#20599 = ORIENTED_EDGE ( 'NONE', *, *, #1256, .F. ) ;
#20600 = CARTESIAN_POINT ( 'NONE',  ( -44.16309181155858710, 473.2448905683720568, -6.410867750099231266 ) ) ;
#20601 = LINE ( 'NONE', #4270, #18969 ) ;
#20602 = CARTESIAN_POINT ( 'NONE',  ( -36.33955658999052218, 403.8698905765656377, 18.47759065022572500 ) ) ;
#20603 = CARTESIAN_POINT ( 'NONE',  ( -42.82802356641965247, 280.7448905765655809, -14.14213562373094746 ) ) ;
#20604 = CARTESIAN_POINT ( 'NONE',  ( -10.20829729246297823, 301.6198905601784759, 7.653668647301790529 ) ) ;
#20605 = CARTESIAN_POINT ( 'NONE',  ( 10.41669750159067220, 217.7548513357008630, 45.00000000000000000 ) ) ;
#20606 = CARTESIAN_POINT ( 'NONE',  ( -24.70764059509556176, 484.8073905765656946, 19.99999999999998934 ) ) ;
#20607 = VECTOR ( 'NONE', #10729, 1000.000000000000000 ) ;
#20608 = CARTESIAN_POINT ( 'NONE',  ( -73.08746600497821078, 600.7448905601785327, 22.98912494155475628 ) ) ;
#20609 = CARTESIAN_POINT ( 'NONE',  ( 20.74841189052422052, 585.7448905601785327, 7.500000000000000000 ) ) ;
#20610 = LINE ( 'NONE', #18656, #4523 ) ;
#20611 = CARTESIAN_POINT ( 'NONE',  ( -35.09675569278794427, 277.2448905683720568, 15.47720386886985366 ) ) ;
#20612 = CARTESIAN_POINT ( 'NONE',  ( -48.68588794268869435, 247.5573905601785043, 3.978247347593168115 ) ) ;
#20613 = CIRCLE ( 'NONE', #17165, 4.999999999999990230 ) ;
#20614 = CARTESIAN_POINT ( 'NONE',  ( -8.685887942688726326, 406.9948905765656377, -2.449293598294705724E-15 ) ) ;
#20615 = CARTESIAN_POINT ( 'NONE',  ( -42.88789093042844058, 436.3073905683720568, 9.489475012073736337 ) ) ;
#20616 = FACE_OUTER_BOUND ( 'NONE', #11554, .T. ) ;
#20617 = CARTESIAN_POINT ( 'NONE',  ( -13.20868407381884779, 269.7448905683720568, 6.410867750099229490 ) ) ;
#20618 = ORIENTED_EDGE ( 'NONE', *, *, #13021, .F. ) ;
#20619 = LINE ( 'NONE', #5795, #19992 ) ;
#20620 = ORIENTED_EDGE ( 'NONE', *, *, #733, .T. ) ;
#20621 = CARTESIAN_POINT ( 'NONE',  ( -45.43829269268872650, 475.3698905683720568, 0.000000000000000000 ) ) ;
#20622 = VECTOR ( 'NONE', #11862, 1000.000000000000000 ) ;
#20623 = ORIENTED_EDGE ( 'NONE', *, *, #9208, .F. ) ;
#20624 = CARTESIAN_POINT ( 'NONE',  ( -11.73070664223726745, 526.0573905765656946, 11.32908994701042005 ) ) ;
#20625 = CARTESIAN_POINT ( 'NONE',  ( -13.20868407381884602, 248.2448905683720000, 6.410867750099229490 ) ) ;
#20626 = ORIENTED_EDGE ( 'NONE', *, *, #9004, .F. ) ;
#20627 = FACE_OUTER_BOUND ( 'NONE', #2191, .T. ) ;
#20628 = AXIS2_PLACEMENT_3D ( 'NONE', #10863, #14243, #7724 ) ;
#20629 = CARTESIAN_POINT ( 'NONE',  ( -48.68588794268872277, 472.3073905765656377, 3.978247347593168115 ) ) ;
#20630 = CARTESIAN_POINT ( 'NONE',  ( 0.05458999538792619344, -1.264741368075137817, 6.499999999999999112 ) ) ;
#20631 = SURFACE_SIDE_STYLE ('',( #7746 ) ) ;
#20632 = DIRECTION ( 'NONE',  ( -0.000000000000000000, 0.000000000000000000, 1.000000000000000000 ) ) ;
#20633 = CARTESIAN_POINT ( 'NONE',  ( -40.53162694259542320, 224.1198905683720000, -11.84573899990672707 ) ) ;
#20634 =( BOUNDED_CURVE ( )  B_SPLINE_CURVE ( 2, ( #15356, #13943, #7205, #20208, #7421, #18677, #10347, #537, #13724, #10559, #2361, #10455, #15455, #2257, #4079, #17075, #8941 ),
 .UNSPECIFIED., .F., .T. ) 
 B_SPLINE_CURVE_WITH_KNOTS ( ( 3, 2, 2, 2, 2, 2, 2, 2, 3 ),
 ( 0.4531250000000002220, 0.4550781250000002220, 0.4570312500000002220, 0.4589843750000002220, 0.4609375000000002220, 0.4628906250000002220, 0.4648437500000002220, 0.4667968750000002220, 0.4687500000000002220 ),
 .UNSPECIFIED. ) 
 CURVE ( )  GEOMETRIC_REPRESENTATION_ITEM ( )  RATIONAL_B_SPLINE_CURVE ( ( 0.9999999999999977796, 0.9807852804032326510, 1.000000000000000000, 0.9807852804032304306, 1.000000000000000000, 0.9807852804032304306, 1.000000000000000000, 0.9807852804032304306, 1.000000000000000000, 0.9807852804032304306, 1.000000000000000000, 0.9807852804032304306, 1.000000000000000000, 0.9807852804032304306, 1.000000000000000000, 0.9807852804032282101, 1.000000000000002220 ) ) 
 REPRESENTATION_ITEM ( '' )  );
#20635 = CARTESIAN_POINT ( 'NONE',  ( -35.09675569278796559, 523.4948905683720568, -15.47720386886985544 ) ) ;
#20636 = LINE ( 'NONE', #19011, #14592 ) ;
#20637 = CARTESIAN_POINT ( 'NONE',  ( -11.93348319268870839, 239.1823905683720284, -3.332260488124732856 ) ) ;
#20638 = CARTESIAN_POINT ( 'NONE',  ( -22.27502019258947286, 328.4948905683720568, 15.47720386886985189 ) ) ;
#20639 = VECTOR ( 'NONE', #13194, 1000.000000000000000 ) ;
#20640 = CARTESIAN_POINT ( 'NONE',  ( 115.7989814974898195, 160.1716627696691830, -20.00000000000000355 ) ) ;
#20641 = CARTESIAN_POINT ( 'NONE',  ( -42.82802356641965247, 303.2448905765656377, 14.14213562373094923 ) ) ;
#20642 = VECTOR ( 'NONE', #17835, 1000.000000000000114 ) ;
#20643 = CARTESIAN_POINT ( 'NONE',  ( -11.93348319268872437, 388.8698905683720000, -2.051577885510841163E-15 ) ) ;
#20644 = EDGE_CURVE ( 'NONE', #1316, #13, #6871, .T. ) ;
#20645 = CARTESIAN_POINT ( 'NONE',  ( -40.01497788969912506, 323.5573905765655809, 16.95518130045146776 ) ) ;
#20646 = CARTESIAN_POINT ( 'NONE',  ( -8.685887942688722774, 381.9323905601784759, 3.978247347593161010 ) ) ;
#20647 = ORIENTED_EDGE ( 'NONE', *, *, #15192, .T. ) ;
#20648 = CARTESIAN_POINT ( 'NONE',  ( -48.68588794268871567, 407.2448905601784759, 0.000000000000000000 ) ) ;
#20649 = ORIENTED_EDGE ( 'NONE', *, *, #14352, .T. ) ;
#20650 = ORIENTED_EDGE ( 'NONE', *, *, #6035, .F. ) ;
#20651 = CARTESIAN_POINT ( 'NONE',  ( -44.16309181155858710, 504.7448905683720000, -6.410867750099231266 ) ) ;
#20652 = DIRECTION ( 'NONE',  ( 1.000000000000000000, 0.000000000000000000, 0.000000000000000000 ) ) ;
#20653 = ORIENTED_EDGE ( 'NONE', *, *, #10446, .F. ) ;
#20654 = CARTESIAN_POINT ( 'NONE',  ( -25.35362745456397349, 298.1823905683720000, 16.75240474999998952 ) ) ;
#20655 = ORIENTED_EDGE ( 'NONE', *, *, #21120, .F. ) ;
#20656 = CARTESIAN_POINT ( 'NONE',  ( -25.35362745456398770, 341.0573905683720000, -16.75240474999999307 ) ) ;
#20657 = CARTESIAN_POINT ( 'NONE',  ( -32.01814843081344719, 341.6823905683720000, -16.75240474999999307 ) ) ;
#20658 = CARTESIAN_POINT ( 'NONE',  ( -36.33955658999050087, 280.1198905765656377, -18.47759065022572855 ) ) ;
#20659 = CARTESIAN_POINT ( 'NONE',  ( -36.33955658999051508, 395.3698905601785327, -18.47759065022572855 ) ) ;
#20660 = CARTESIAN_POINT ( 'NONE',  ( -28.68588794268869790, 246.3698905683720000, 16.75240474999999307 ) ) ;
#20661 = DIRECTION ( 'NONE',  ( 0.000000000000000000, 1.000000000000000000, 0.000000000000000000 ) ) ;
#20662 = CARTESIAN_POINT ( 'NONE',  ( -19.19641293061498999, 391.9323905683720000, -14.20200298773971603 ) ) ;
#20663 = EDGE_CURVE ( 'NONE', #18143, #10958, #15014, .T. ) ;
#20664 = LINE ( 'NONE', #4227, #11655 ) ;
#20665 = FACE_OUTER_BOUND ( 'NONE', #15156, .T. ) ;
#20666 = CARTESIAN_POINT ( 'NONE',  ( -17.35679799567828141, 243.8073905601784759, -16.95518130045146421 ) ) ;
#20667 = CARTESIAN_POINT ( 'NONE',  ( -42.88789093042844058, 442.9323905683721136, -9.489475012073736337 ) ) ;
#20668 = EDGE_LOOP ( 'NONE', ( #3836, #3565, #17280, #14286 ) ) ;
#20669 = CARTESIAN_POINT ( 'NONE',  ( -32.66413529028188378, 439.4323905601785327, 19.99999999999999289 ) ) ;
#20670 = ORIENTED_EDGE ( 'NONE', *, *, #7618, .T. ) ;
#20671 = CARTESIAN_POINT ( 'NONE',  ( 4.700000000000000178, 5.629165124598848102, 3.250000000000005773 ) ) ;
#20672 = VERTEX_POINT ( 'NONE', #5355 ) ;
#20673 = ORIENTED_EDGE ( 'NONE', *, *, #3842, .F. ) ;
#20674 = CARTESIAN_POINT ( 'NONE',  ( 4.700000000000000178, 6.500000000000000888, 0.000000000000000000 ) ) ;
#20675 = CARTESIAN_POINT ( 'NONE',  ( -48.68588794268870146, 316.9323905601784759, -3.978247347593158345 ) ) ;
#20676 = CARTESIAN_POINT ( 'NONE',  ( -11.93348319268871549, 298.5573905683720000, 3.332260488124728415 ) ) ;
#20677 = EDGE_CURVE ( 'NONE', #12627, #8982, #19098, .T. ) ;
#20678 = CARTESIAN_POINT ( 'NONE',  ( -44.16309181155857289, 364.7448905683720568, -6.410867750099231266 ) ) ;
#20679 = CARTESIAN_POINT ( 'NONE',  ( 115.7989814974898195, 160.1716627696692683, 40.00000000000000000 ) ) ;
#20680 = CARTESIAN_POINT ( 'NONE',  ( -36.33955658999052929, 530.1198905765655809, -18.47759065022572855 ) ) ;
#20681 = CARTESIAN_POINT ( 'NONE',  ( -45.43829269268871229, 404.1823905683720568, 3.332260488124734632 ) ) ;
#20682 = CARTESIAN_POINT ( 'NONE',  ( -25.35362745456396638, 238.1823905683720852, 16.75240474999998952 ) ) ;
#20683 = CARTESIAN_POINT ( 'NONE',  ( -45.43829269268871940, 403.8698905683720000, 0.000000000000000000 ) ) ;
#20684 = ITEM_DEFINED_TRANSFORMATION ( 'NONE', 'NONE', #3144,  #12794 ) ;
#20685 = AXIS2_PLACEMENT_3D ( 'NONE', #12621, #3090, #8046 ) ;
#20686 = CARTESIAN_POINT ( 'NONE',  ( -10.20829729246298356, 347.6198905765656377, -7.653668647301794969 ) ) ;
#20687 = CARTESIAN_POINT ( 'NONE',  ( -11.73070664223724613, 323.1823905601784190, -11.32908994701042538 ) ) ;
#20688 = CARTESIAN_POINT ( 'NONE',  ( -38.17536295476244135, 315.4323905683720000, 14.20200298773971781 ) ) ;
#20689 = SHAPE_REPRESENTATION_RELATIONSHIP ( 'NONE' , 'NONE' ,  #21199, #7644 ) ;
#20690 = CARTESIAN_POINT ( 'NONE',  ( -25.35362745456400191, 462.5573905683720000, -16.75240474999999307 ) ) ;
#20691 = EDGE_CURVE ( 'NONE', #5267, #6197, #2162, .T. ) ;
#20692 = CARTESIAN_POINT ( 'NONE',  ( -17.35679799567829917, 460.6823905601785327, 16.95518130045146421 ) ) ;
#20693 = CARTESIAN_POINT ( 'NONE',  ( -42.87301415892787304, 204.0033847496196699, -4.870997244581529273 ) ) ;
#20694 = CARTESIAN_POINT ( 'NONE',  ( -123.2946569474810161, 30.52886280891152282, 20.57735571454641388 ) ) ;
#20695 = CARTESIAN_POINT ( 'NONE',  ( -22.27502019258948707, 372.2448905683720000, -15.47720386886985544 ) ) ;
#20696 = CARTESIAN_POINT ( 'NONE',  ( -40.53162694259545162, 502.6198905683720568, -11.84573899990672707 ) ) ;
#20697 = CARTESIAN_POINT ( 'NONE',  ( -28.68588794268872988, 499.7448905601785327, 19.99999999999999289 ) ) ;
#20698 = CARTESIAN_POINT ( 'NONE',  ( -40.53162694259543741, 342.6198905683720000, -11.84573899990672707 ) ) ;
#20699 = AXIS2_PLACEMENT_3D ( 'NONE', #6202, #9023, #5778 ) ;
#20700 = ORIENTED_EDGE ( 'NONE', *, *, #9348, .T. ) ;
#20701 = CARTESIAN_POINT ( 'NONE',  ( -32.01814843081346140, 496.0573905683720568, 16.75240474999999307 ) ) ;
#20702 = VERTEX_POINT ( 'NONE', #6657 ) ;
#20703 = LINE ( 'NONE', #12489, #18773 ) ;
#20704 = CARTESIAN_POINT ( 'NONE',  ( -45.43829269268871940, 425.6823905683720568, 3.332260488124734632 ) ) ;
#20705 = CARTESIAN_POINT ( 'NONE',  ( -48.68588794268870856, 331.9948905765656377, 0.000000000000000000 ) ) ;
#20706 = AXIS2_PLACEMENT_3D ( 'NONE', #1562, #11179, #17673 ) ;
#20707 = CARTESIAN_POINT ( 'NONE',  ( -28.68588794268872633, 230.8848358243226073, 0.000000000000000000 ) ) ;
#20708 = CARTESIAN_POINT ( 'NONE',  ( -11.93348319268873325, 458.8698905683720000, -2.051577885510841163E-15 ) ) ;
#20709 = ORIENTED_EDGE ( 'NONE', *, *, #20775, .F. ) ;
#20710 = CARTESIAN_POINT ( 'NONE',  ( -25.35362745456399480, 466.6823905683720000, 16.75240474999998952 ) ) ;
#20711 = CARTESIAN_POINT ( 'NONE',  ( -42.82802356641964536, 248.4948905601784759, 14.14213562373094923 ) ) ;
#20712 = CARTESIAN_POINT ( 'NONE',  ( -8.685887942688726326, 396.6823905765656946, 3.978247347593161010 ) ) ;
#20713 = CARTESIAN_POINT ( 'NONE',  ( -47.16347859291443712, 281.3698905765656377, -7.653668647301793193 ) ) ;
#20714 = CARTESIAN_POINT ( 'NONE',  ( -8.685887942688724550, 366.9948905765655809, -2.449293598294705724E-15 ) ) ;
#20715 = CARTESIAN_POINT ( 'NONE',  ( -8.685887942688742314, 573.2448905601785327, 2.449293598294706119E-15 ) ) ;
#20716 = CARTESIAN_POINT ( 'NONE',  ( -17.35679799567830273, 485.4323905765656946, 16.95518130045146421 ) ) ;
#20717 = CARTESIAN_POINT ( 'NONE',  ( -28.68588794268874054, 333.8848358243226357, 40.00000000000000000 ) ) ;
#20718 =( LENGTH_UNIT ( ) NAMED_UNIT ( * ) SI_UNIT ( .MILLI., .METRE. ) );
#20719 = CARTESIAN_POINT ( 'NONE',  ( -10.20829729246299244, 421.6198905601785327, 7.653668647301790529 ) ) ;
#20720 = EDGE_CURVE ( 'NONE', #1338, #10157, #3428, .T. ) ;
#20721 = CARTESIAN_POINT ( 'NONE',  ( -13.20868407381884779, 279.7448905683720568, 6.410867750099229490 ) ) ;
#20722 = EDGE_CURVE ( 'NONE', #3061, #2116, #13279, .T. ) ;
#20723 = CARTESIAN_POINT ( 'NONE',  ( -48.68588794268869435, 257.2448905601784759, 0.000000000000000000 ) ) ;
#20724 = DIRECTION ( 'NONE',  ( 0.000000000000000000, -1.000000000000000000, 0.000000000000000000 ) ) ;
#20725 = CARTESIAN_POINT ( 'NONE',  ( -35.09675569278795138, 423.4948905683720568, -15.47720386886985544 ) ) ;
#20726 = DIRECTION ( 'NONE',  ( -1.191790137725560488E-16, 1.000000000000000000, -0.000000000000000000 ) ) ;
#20727 = CARTESIAN_POINT ( 'NONE',  ( -44.16309181155855867, 244.7448905683720000, -6.410867750099231266 ) ) ;
#20728 = ORIENTED_EDGE ( 'NONE', *, *, #15717, .F. ) ;
#20729 = EDGE_LOOP ( 'NONE', ( #9512, #7461, #8047, #5033, #20547, #13510, #262, #5215, #18636, #5265, #3982, #6967 ) ) ;
#20730 = LINE ( 'NONE', #14363, #8754 ) ;
#20731 = ORIENTED_EDGE ( 'NONE', *, *, #1759, .F. ) ;
#20732 = CARTESIAN_POINT ( 'NONE',  ( -11.93348319268873503, 480.6823905683720568, -3.332260488124732856 ) ) ;
#20733 = ADVANCED_FACE ( 'NONE', ( #1820 ), #6978, .F. ) ;
#20734 = VERTEX_POINT ( 'NONE', #3531 ) ;
#20735 = CARTESIAN_POINT ( 'NONE',  ( -42.82802356641965957, 365.9948905601784759, -14.14213562373094746 ) ) ;
#20736 = CARTESIAN_POINT ( 'NONE',  ( -35.09675569278793716, 235.7448905683720000, 15.47720386886985366 ) ) ;
#20737 = ORIENTED_EDGE ( 'NONE', *, *, #16367, .T. ) ;
#20738 = CARTESIAN_POINT ( 'NONE',  ( -22.27502019258950483, 520.7448905683720568, -15.47720386886985544 ) ) ;
#20739 = DIRECTION ( 'NONE',  ( -1.191790137725560488E-16, 1.000000000000000000, -0.000000000000000000 ) ) ;
#20740 = ADVANCED_FACE ( 'NONE', ( #19864 ), #16632, .F. ) ;
#20741 = CARTESIAN_POINT ( 'NONE',  ( -45.64106924314020119, 461.0573905765656377, -11.32908994701042715 ) ) ;
#20742 = CARTESIAN_POINT ( 'NONE',  ( 115.7989814974898337, 152.5259582928263740, -20.00000000000000355 ) ) ;
#20743 = DIRECTION ( 'NONE',  ( 0.000000000000000000, 0.000000000000000000, -1.000000000000000000 ) ) ;
#20744 = CARTESIAN_POINT ( 'NONE',  ( -28.68588794268875475, 600.7448905601785327, 0.000000000000000000 ) ) ;
#20745 = CARTESIAN_POINT ( 'NONE',  ( -32.01814843081346851, 517.5573905683720568, 16.75240474999999307 ) ) ;
#20746 = CARTESIAN_POINT ( 'NONE',  ( 91.21585410611801592, 56.85652257517428865, -94.99999999999994316 ) ) ;
#20747 = CARTESIAN_POINT ( 'NONE',  ( -42.88789093042841927, 254.8073905683720284, 9.489475012073736337 ) ) ;
#20748 = CARTESIAN_POINT ( 'NONE',  ( -35.09675569278794427, 333.4948905683720568, -15.47720386886985544 ) ) ;
#20749 = ADVANCED_FACE ( 'NONE', ( #16843 ), #13385, .F. ) ;
#20750 = CARTESIAN_POINT ( 'NONE',  ( -48.68588794268887909, 467.5573905601785327, 3.978247347592795524 ) ) ;
#20751 = VECTOR ( 'NONE', #382, 1000.000000000000000 ) ;
#20752 = CARTESIAN_POINT ( 'NONE',  ( -8.685887942688717445, 306.9948905765655809, -2.449293598294705724E-15 ) ) ;
#20753 = VECTOR ( 'NONE', #16383, 1000.000000000000000 ) ;
#20754 = CARTESIAN_POINT ( 'NONE',  ( -22.27502019258949062, 390.7448905683720000, -15.47720386886985544 ) ) ;
#20755 = TOROIDAL_SURFACE ( 'NONE', #18668, 4.400000000000000355, 0.4000000000000000222 ) ;
#20756 = FACE_OUTER_BOUND ( 'NONE', #7937, .T. ) ;
#20757 = AXIS2_PLACEMENT_3D ( 'NONE', #9861, #1670, #6512 ) ;
#20758 = CARTESIAN_POINT ( 'NONE',  ( -48.68588794268870856, 387.2448905601784759, 0.000000000000000000 ) ) ;
#20759 = ORIENTED_EDGE ( 'NONE', *, *, #7140, .T. ) ;
#20760 = CARTESIAN_POINT ( 'NONE',  ( -28.68588794268874764, 575.7448905601785327, 0.000000000000000000 ) ) ;
#20761 = EDGE_LOOP ( 'NONE', ( #17306, #16238, #9192, #14897 ) ) ;
#20762 = ORIENTED_EDGE ( 'NONE', *, *, #20866, .T. ) ;
#20763 = CARTESIAN_POINT ( 'NONE',  ( -32.01814843081346140, 497.5573905683720568, 16.75240474999999307 ) ) ;
#20764 = CARTESIAN_POINT ( 'NONE',  ( -10.20829729246297823, 296.3698905765655809, 7.653668647301790529 ) ) ;
#20765 = ORIENTED_EDGE ( 'NONE', *, *, #10876, .T. ) ;
#20766 =( BOUNDED_CURVE ( )  B_SPLINE_CURVE ( 2, ( #16696, #5314, #11915, #1885, #2085, #5418, #13986, #12131, #10496, #10819, #3798, #4008, #17117, #681, #5846, #10602, #18933 ),
 .UNSPECIFIED., .F., .T. ) 
 B_SPLINE_CURVE_WITH_KNOTS ( ( 3, 2, 2, 2, 2, 2, 2, 2, 3 ),
 ( 0.6093750000000002220, 0.6113281250000002220, 0.6132812500000002220, 0.6152343750000002220, 0.6171875000000002220, 0.6191406250000002220, 0.6210937500000002220, 0.6230468750000002220, 0.6250000000000002220 ),
 .UNSPECIFIED. ) 
 CURVE ( )  GEOMETRIC_REPRESENTATION_ITEM ( )  RATIONAL_B_SPLINE_CURVE ( ( 0.9999999999999977796, 0.9807852804032326510, 1.000000000000000000, 0.9807852804032304306, 1.000000000000000000, 0.9807852804032304306, 1.000000000000000000, 0.9807852804032304306, 1.000000000000000000, 0.9807852804032304306, 1.000000000000000000, 0.9807852804032304306, 1.000000000000000000, 0.9807852804032304306, 1.000000000000000000, 0.9807852804032282101, 1.000000000000002220 ) ) 
 REPRESENTATION_ITEM ( '' )  );
#20767 = CARTESIAN_POINT ( 'NONE',  ( -28.68588794268870501, 307.8698905683720000, 16.75240474999999307 ) ) ;
#20768 = CARTESIAN_POINT ( 'NONE',  ( -16.84014894278200813, 501.6198905683720000, -11.84573899990672707 ) ) ;
#20769 = EDGE_LOOP ( 'NONE', ( #3934, #17171 ) ) ;
#20770 = CARTESIAN_POINT ( 'NONE',  ( -45.43829269268870519, 334.1823905683720000, 3.332260488124734632 ) ) ;
#20771 = CARTESIAN_POINT ( 'NONE',  ( -45.43829269268871229, 343.8698905683720000, 0.000000000000000000 ) ) ;
#20772 = CARTESIAN_POINT ( 'NONE',  ( -11.73070664223723547, 276.0573905765656377, 11.32908994701042005 ) ) ;
#20773 = VECTOR ( 'NONE', #4135, 1000.000000000000114 ) ;
#20774 = DIRECTION ( 'NONE',  ( -1.191790137725560488E-16, 1.000000000000000000, -0.000000000000000000 ) ) ;
#20775 = EDGE_CURVE ( 'NONE', #7989, #2589, #3551, .T. ) ;
#20776 = CARTESIAN_POINT ( 'NONE',  ( -19.19641293061496512, 237.3073905683720284, 14.20200298773971426 ) ) ;
#20777 = APPLICATION_CONTEXT ( 'automotive_design' ) ;
#20778 = CARTESIAN_POINT ( 'NONE',  ( -44.16309181155857289, 395.9948905683720568, 6.410867750099241924 ) ) ;
#20779 = CARTESIAN_POINT ( 'NONE',  ( -28.68588794268872633, 333.8848358243226357, 0.000000000000000000 ) ) ;
#20780 = DIRECTION ( 'NONE',  ( 0.000000000000000000, -0.000000000000000000, -1.000000000000000000 ) ) ;
#20781 = CARTESIAN_POINT ( 'NONE',  ( -45.64106924314016567, 246.3073905601784759, -11.32908994701042538 ) ) ;
#20782 = CARTESIAN_POINT ( 'NONE',  ( -44.16309181155857999, 443.2448905683720000, -6.410867750099231266 ) ) ;
#20783 = ORIENTED_EDGE ( 'NONE', *, *, #13548, .F. ) ;
#20784 = CARTESIAN_POINT ( 'NONE',  ( -17.35679799567830983, 453.8073905601784759, -16.95518130045146421 ) ) ;
#20785 = EDGE_LOOP ( 'NONE', ( #8055, #21124, #4174 ) ) ;
#20786 = EDGE_LOOP ( 'NONE', ( #13792, #4296, #2462, #20311 ) ) ;
#20787 = ORIENTED_EDGE ( 'NONE', *, *, #19806, .F. ) ;
#20788 = DIRECTION ( 'NONE',  ( 0.000000000000000000, 0.000000000000000000, -1.000000000000000000 ) ) ;
#20789 = VECTOR ( 'NONE', #20652, 1000.000000000000000 ) ;
#20790 = CARTESIAN_POINT ( 'NONE',  ( -24.70764059509554755, 330.0573905601785327, 19.99999999999998934 ) ) ;
#20791 = ADVANCED_FACE ( 'NONE', ( #11855 ), #20292, .T. ) ;
#20792 = CARTESIAN_POINT ( 'NONE',  ( -32.01814843081344719, 363.1823905683720568, -16.75240474999999307 ) ) ;
#20793 = CARTESIAN_POINT ( 'NONE',  ( -47.16347859291443001, 227.8698905601784759, 7.653668647301805628 ) ) ;
#20794 = CARTESIAN_POINT ( 'NONE',  ( -14.54375231895778597, 515.7448905765655809, 14.14213562373094568 ) ) ;
#20795 = CARTESIAN_POINT ( 'NONE',  ( -28.68588794268871567, 396.3698905683720000, 16.75240474999999307 ) ) ;
#20796 = CARTESIAN_POINT ( 'NONE',  ( -11.93348319268870661, 240.3698905683720568, -2.051577885510841163E-15 ) ) ;
#20797 = CARTESIAN_POINT ( 'NONE',  ( -13.20868407381886556, 399.4948905683720000, -6.410867750099233042 ) ) ;
#20798 = CARTESIAN_POINT ( 'NONE',  ( -24.70764059509555111, 344.8073905765656377, 19.99999999999998934 ) ) ;
#20799 = CARTESIAN_POINT ( 'NONE',  ( -40.01497788969913216, 325.6823905601784759, -16.95518130045146421 ) ) ;
#20800 = CARTESIAN_POINT ( 'NONE',  ( -35.09675569278793716, 311.9948905683720568, -15.47720386886985544 ) ) ;
#20801 = CARTESIAN_POINT ( 'NONE',  ( -28.68588794268872988, 462.8698905683720000, -16.75240474999999307 ) ) ;
#20802 = LINE ( 'NONE', #6073, #19568 ) ;
#20803 = DIRECTION ( 'NONE',  ( 1.191790137725560488E-16, -1.000000000000000000, -0.000000000000000000 ) ) ;
#20804 = DIRECTION ( 'NONE',  ( 0.000000000000000000, 0.000000000000000000, -1.000000000000000000 ) ) ;
#20805 =( GEOMETRIC_REPRESENTATION_CONTEXT ( 3 ) GLOBAL_UNCERTAINTY_ASSIGNED_CONTEXT ( ( #13956 ) ) GLOBAL_UNIT_ASSIGNED_CONTEXT ( ( #16948, #4939, #19755 ) ) REPRESENTATION_CONTEXT ( 'NONE', 'WORKASPACE' ) );
#20806 = EDGE_CURVE ( 'NONE', #11682, #6477, #14270, .T. ) ;
#20807 = CARTESIAN_POINT ( 'NONE',  ( -16.84014894278199037, 361.6198905683720000, -11.84573899990672707 ) ) ;
#20808 = CARTESIAN_POINT ( 'NONE',  ( -35.09675569278795848, 501.9948905683720000, -15.47720386886985544 ) ) ;
#20809 = CARTESIAN_POINT ( 'NONE',  ( -40.01497788969914637, 498.8073905601784759, 16.95518130045146776 ) ) ;
#20810 = CARTESIAN_POINT ( 'NONE',  ( -16.84014894278198682, 330.1198905683720568, -11.84573899990672707 ) ) ;
#20811 = ORIENTED_EDGE ( 'NONE', *, *, #5051, .F. ) ;
#20812 = CARTESIAN_POINT ( 'NONE',  ( -22.27502019258950128, 500.7448905683720000, -15.47720386886985544 ) ) ;
#20813 = ORIENTED_EDGE ( 'NONE', *, *, #12784, .F. ) ;
#20814 = AXIS2_PLACEMENT_3D ( 'NONE', #10119, #16741, #15120 ) ;
#20815 = CARTESIAN_POINT ( 'NONE',  ( -8.685887942688893304, 316.6823905765655809, 3.978247347593586447 ) ) ;
#20816 = EDGE_CURVE ( 'NONE', #15898, #19525, #15649, .T. ) ;
#20817 = CARTESIAN_POINT ( 'NONE',  ( -11.93348319268872793, 420.3698905683720568, -2.051577885510841163E-15 ) ) ;
#20818 = CARTESIAN_POINT ( 'NONE',  ( -11.73070664223724968, 396.0573905765655809, 11.32908994701042005 ) ) ;
#20819 = LINE ( 'NONE', #4899, #17972 ) ;
#20820 = CARTESIAN_POINT ( 'NONE',  ( -13.20868407381887266, 459.4948905683720568, -6.410867750099233042 ) ) ;
#20821 = VECTOR ( 'NONE', #861, 1000.000000000000000 ) ;
#20822 = VERTEX_POINT ( 'NONE', #2236 ) ;
#20823 = CARTESIAN_POINT ( 'NONE',  ( -22.27502019258948707, 456.9948905683720000, 15.47720386886985189 ) ) ;
#20824 = CARTESIAN_POINT ( 'NONE',  ( -8.685887942688708563, 242.2448905601785043, -2.449293598294705724E-15 ) ) ;
#20825 = CARTESIAN_POINT ( 'NONE',  ( -10.20829729246299067, 407.6198905765656377, -7.653668647301794969 ) ) ;
#20826 = DIRECTION ( 'NONE',  ( 1.191790137725560488E-16, -1.000000000000000000, -0.000000000000000000 ) ) ;
#20827 = CARTESIAN_POINT ( 'NONE',  ( -123.2946569474810019, -343.0245277843623057, -20.57735571454641388 ) ) ;
#20828 = DIRECTION ( 'NONE',  ( -0.000000000000000000, -0.000000000000000000, 1.000000000000000000 ) ) ;
#20829 = DIRECTION ( 'NONE',  ( -0.000000000000000000, -1.000000000000000000, -0.000000000000000000 ) ) ;
#20830 = DIRECTION ( 'NONE',  ( 1.000000000000000000, 1.250996701150283068E-16, -0.000000000000000000 ) ) ;
#20831 = CARTESIAN_POINT ( 'NONE',  ( -17.35679799567829207, 343.8073905601785327, -16.95518130045146421 ) ) ;
#20832 = CIRCLE ( 'NONE', #4918, 3.309499999999999886 ) ;
#20833 = CARTESIAN_POINT ( 'NONE',  ( -8.685887942688708563, 242.5573905601784759, -3.978247347593165895 ) ) ;
#20834 = CARTESIAN_POINT ( 'NONE',  ( 5.074999999999999289, 3.752776749732560368, -6.499999999999999112 ) ) ;
#20835 = CARTESIAN_POINT ( 'NONE',  ( -42.88789093042844058, 426.3073905683720568, 9.489475012073736337 ) ) ;
#20836 = CARTESIAN_POINT ( 'NONE',  ( -28.68588794268869790, 213.9102039777116602, 0.000000000000000000 ) ) ;
#20837 = CARTESIAN_POINT ( 'NONE',  ( -45.43829269268869808, 255.3698905683720000, 0.000000000000000000 ) ) ;
#20838 = VERTEX_POINT ( 'NONE', #9243 ) ;
#20839 = ORIENTED_EDGE ( 'NONE', *, *, #19162, .F. ) ;
#20840 = DIRECTION ( 'NONE',  ( -1.191790137725560488E-16, 1.000000000000000000, 0.000000000000000000 ) ) ;
#20841 = EDGE_LOOP ( 'NONE', ( #17693, #19632, #12911 ) ) ;
#20842 = CARTESIAN_POINT ( 'NONE',  ( -14.48388495494901029, 469.4323905683720568, 9.489475012073731008 ) ) ;
#20843 = VECTOR ( 'NONE', #2507, 1000.000000000000000 ) ;
#20844 = EDGE_LOOP ( 'NONE', ( #18510, #10205 ) ) ;
#20845 = DIRECTION ( 'NONE',  ( -0.8090169943749473402, 0.000000000000000000, 0.5877852522924733591 ) ) ;
#20846 = CARTESIAN_POINT ( 'NONE',  ( -38.17536295476243424, 245.4323905683720000, 14.20200298773971781 ) ) ;
#20847 = VECTOR ( 'NONE', #3137, 1000.000000000000114 ) ;
#20848 = ORIENTED_EDGE ( 'NONE', *, *, #3225, .F. ) ;
#20849 = CARTESIAN_POINT ( 'NONE',  ( -25.35362745456399836, 516.6823905683720568, 16.75240474999998952 ) ) ;
#20850 = DIRECTION ( 'NONE',  ( 0.8090169943749473402, 0.000000000000000000, -0.5877852522924733591 ) ) ;
#20851 = CARTESIAN_POINT ( 'NONE',  ( -14.54375231895777887, 455.7448905765656377, 14.14213562373094568 ) ) ;
#20852 = CARTESIAN_POINT ( 'NONE',  ( 1.863472483959460130E-17, -0.6346842323199924918, 6.499999999999999112 ) ) ;
#20853 = FILL_AREA_STYLE ('',( #15995 ) ) ;
#20854 = CARTESIAN_POINT ( 'NONE',  ( -28.68588794268872633, 454.7448905601784759, -19.99999999999999289 ) ) ;
#20855 = CARTESIAN_POINT ( 'NONE',  ( -22.27502019258947286, 232.2448905683720000, -15.47720386886985544 ) ) ;
#20856 = CARTESIAN_POINT ( 'NONE',  ( 0.4037800551813739425, 7.199367570657606130, 0.5303295852573159941 ) ) ;
#20857 = CARTESIAN_POINT ( 'NONE',  ( -32.01814843081343298, 226.0573905683720568, 16.75240474999999307 ) ) ;
#20858 = CARTESIAN_POINT ( 'NONE',  ( -38.17536295476245556, 333.8073905683720000, -14.20200298773971426 ) ) ;
#20859 = EDGE_CURVE ( 'NONE', #3036, #16900, #17019, .T. ) ;
#20860 = AXIS2_PLACEMENT_3D ( 'NONE', #20520, #18882, #4394 ) ;
#20861 = CARTESIAN_POINT ( 'NONE',  ( -10.20829729246299777, 471.6198905601784759, 7.653668647301790529 ) ) ;
#20862 = LINE ( 'NONE', #12641, #9896 ) ;
#20863 = ADVANCED_FACE ( 'NONE', ( #15541 ), #1046, .F. ) ;
#20864 = AXIS2_PLACEMENT_3D ( 'NONE', #8136, #21140, #21353 ) ;
#20865 = CARTESIAN_POINT ( 'NONE',  ( -42.88789093042842637, 304.4323905683720000, -9.489475012073736337 ) ) ;
#20866 = EDGE_CURVE ( 'NONE', #827, #11603, #8726, .T. ) ;
#20867 = CARTESIAN_POINT ( 'NONE',  ( -16.84014894278199392, 390.1198905683720000, -11.84573899990672707 ) ) ;
#20868 = LINE ( 'NONE', #14060, #1884 ) ;
#20869 = CARTESIAN_POINT ( 'NONE',  ( -24.70764059509555466, 390.0573905601784759, 19.99999999999998934 ) ) ;
#20870 = PLANE ( 'NONE',  #4271 ) ;
#20871 = VERTEX_POINT ( 'NONE', #13805 ) ;
#20872 = EDGE_LOOP ( 'NONE', ( #20593, #17567, #2566, #16566, #5716 ) ) ;
#20873 = CARTESIAN_POINT ( 'NONE',  ( -13.20868407381887799, 500.9948905683721136, -6.410867750099233042 ) ) ;
#20874 = DIRECTION ( 'NONE',  ( -1.191790137725560488E-16, 1.000000000000000000, -0.000000000000000000 ) ) ;
#20875 = ORIENTED_EDGE ( 'NONE', *, *, #6033, .T. ) ;
#20876 = EDGE_CURVE ( 'NONE', #14922, #13587, #20376, .T. ) ;
#20877 = CARTESIAN_POINT ( 'NONE',  ( -45.43829269268870519, 305.6823905683720000, 3.332260488124734632 ) ) ;
#20878 = CARTESIAN_POINT ( 'NONE',  ( -32.01814843081344009, 326.0573905683720000, 16.75240474999999307 ) ) ;
#20879 = AXIS2_PLACEMENT_3D ( 'NONE', #11492, #14969, #18090 ) ;
#20880 = CARTESIAN_POINT ( 'NONE',  ( -8.685887942688712116, 267.3073905765655809, -3.978247347593165895 ) ) ;
#20881 = CARTESIAN_POINT ( 'NONE',  ( -22.27502019258946220, 236.9948905683720284, 15.47720386886985189 ) ) ;
#20882 = CARTESIAN_POINT ( 'NONE',  ( -45.43829269268871229, 405.6823905683720568, 3.332260488124734632 ) ) ;
#20883 = DIRECTION ( 'NONE',  ( 0.1337298367054296222, -0.9910178256594273094, 0.000000000000000000 ) ) ;
#20884 = DIRECTION ( 'NONE',  ( 0.000000000000000000, 0.5000000000000018874, 0.8660254037844375974 ) ) ;
#20885 = CARTESIAN_POINT ( 'NONE',  ( -8.685887942688708563, 242.2448905601785043, -2.449293598294705724E-15 ) ) ;
#20886 = CARTESIAN_POINT ( 'NONE',  ( -38.17536295476245556, 435.4323905683720568, 14.20200298773971781 ) ) ;
#20887 = ORIENTED_EDGE ( 'NONE', *, *, #12205, .T. ) ;
#20888 =( BOUNDED_CURVE ( )  B_SPLINE_CURVE ( 2, ( #8945, #14160, #18681, #17078, #2472, #643, #5920, #12529, #2261, #10889, #13947, #8839, #9053, #7209, #20425, #14052, #3868 ),
 .UNSPECIFIED., .F., .T. ) 
 B_SPLINE_CURVE_WITH_KNOTS ( ( 3, 2, 2, 2, 2, 2, 2, 2, 3 ),
 ( 0.4843750000000002220, 0.4863281250000002220, 0.4882812500000002220, 0.4902343750000002220, 0.4921875000000002220, 0.4941406250000002220, 0.4960937500000002220, 0.4980468750000002220, 0.5000000000000002220 ),
 .UNSPECIFIED. ) 
 CURVE ( )  GEOMETRIC_REPRESENTATION_ITEM ( )  RATIONAL_B_SPLINE_CURVE ( ( 0.9999999999999977796, 0.9807852804032326510, 1.000000000000000000, 0.9807852804032304306, 1.000000000000000000, 0.9807852804032304306, 1.000000000000000000, 0.9807852804032304306, 1.000000000000000000, 0.9807852804032304306, 1.000000000000000000, 0.9807852804032304306, 1.000000000000000000, 0.9807852804032304306, 1.000000000000000000, 0.9807852804032282101, 1.000000000000002220 ) ) 
 REPRESENTATION_ITEM ( '' )  );
#20889 = CARTESIAN_POINT ( 'NONE',  ( -24.70764059509556176, 440.0573905601785327, 19.99999999999998934 ) ) ;
#20890 = ORIENTED_EDGE ( 'NONE', *, *, #21136, .F. ) ;
#20891 = ORIENTED_EDGE ( 'NONE', *, *, #522, .F. ) ;
#20892 = VERTEX_POINT ( 'NONE', #12502 ) ;
#20893 = DIRECTION ( 'NONE',  ( 0.000000000000000000, 0.000000000000000000, -1.000000000000000000 ) ) ;
#20894 = CARTESIAN_POINT ( 'NONE',  ( -10.20829729246298179, 332.8698905601785327, -7.653668647301794969 ) ) ;
#20895 = CARTESIAN_POINT ( 'NONE',  ( -13.20868407381886200, 370.9948905683720568, -6.410867750099233042 ) ) ;
#20896 = DIRECTION ( 'NONE',  ( -0.000000000000000000, -0.000000000000000000, 1.000000000000000000 ) ) ;
#20897 = CARTESIAN_POINT ( 'NONE',  ( -47.16347859291446554, 512.6198905765656946, 7.653668647301805628 ) ) ;
#20898 = CARTESIAN_POINT ( 'NONE',  ( -25.35362745456399480, 381.0573905683719431, -16.75240474999999307 ) ) ;
#20899 = CARTESIAN_POINT ( 'NONE',  ( -25.35362745456397704, 242.5573905683720000, -16.75240474999999307 ) ) ;
#20900 = CARTESIAN_POINT ( 'NONE',  ( -11.93348319268872615, 398.5573905683720568, 3.332260488124728859 ) ) ;
#20901 = CARTESIAN_POINT ( 'NONE',  ( -28.68588794268871212, 319.4948905765656377, -19.99999999999999289 ) ) ;
#20902 = DIRECTION ( 'NONE',  ( 1.000000000000000000, 0.000000000000000000, 0.000000000000000000 ) ) ;
#20903 = CARTESIAN_POINT ( 'NONE',  ( -25.35362745456397349, 306.6823905683720000, 16.75240474999998952 ) ) ;
#20904 = SHAPE_REPRESENTATION_RELATIONSHIP ( 'NONE' , 'NONE' ,  #7793, #7899 ) ;
#20905 = CARTESIAN_POINT ( 'NONE',  ( -13.20868407381886911, 449.7448905683720000, 6.410867750099229490 ) ) ;
#20906 = CARTESIAN_POINT ( 'NONE',  ( -162.2727221670389781, 30.52886280891152282, 0.000000000000000000 ) ) ;
#20907 = CARTESIAN_POINT ( 'NONE',  ( -42.82802356641965957, 368.4948905601784759, 14.14213562373094923 ) ) ;
#20908 = DIRECTION ( 'NONE',  ( 0.000000000000000000, -1.000000000000000000, 0.000000000000000000 ) ) ;
#20909 = EDGE_CURVE ( 'NONE', #18908, #13314, #2549, .T. ) ;
#20910 = CARTESIAN_POINT ( 'NONE',  ( -11.93348319268872260, 360.0573905683719431, 3.332260488124728415 ) ) ;
#20911 = CARTESIAN_POINT ( 'NONE',  ( -14.48388495494901562, 497.9323905683720568, 9.489475012073732785 ) ) ;
#20912 = CARTESIAN_POINT ( 'NONE',  ( -14.54375231895778775, 503.4948905601784759, -14.14213562373094746 ) ) ;
#20913 = CARTESIAN_POINT ( 'NONE',  ( -11.93348319268871904, 328.5573905683720568, 3.332260488124728415 ) ) ;
#20914 = ORIENTED_EDGE ( 'NONE', *, *, #557, .T. ) ;
#20915 = CARTESIAN_POINT ( 'NONE',  ( 0.000000000000000000, 5.629165124598846326, -3.250000000000007550 ) ) ;
#20916 = VERTEX_POINT ( 'NONE', #5677 ) ;
#20917 = EDGE_CURVE ( 'NONE', #20009, #2721, #12176, .T. ) ;
#20918 = CARTESIAN_POINT ( 'NONE',  ( -74.06037022053952512, 10.52886280891152104, 40.00000000000000000 ) ) ;
#20919 = CARTESIAN_POINT ( 'NONE',  ( -19.19641293061498644, 428.8073905683720000, 14.20200298773971426 ) ) ;
#20920 = CARTESIAN_POINT ( 'NONE',  ( -8.685887942688911068, 446.6823905765656377, 3.978247347593586447 ) ) ;
#20921 = DIRECTION ( 'NONE',  ( -0.7071067811865530128, 8.659560562354868763E-17, -0.7071067811865421326 ) ) ;
#20922 = CARTESIAN_POINT ( 'NONE',  ( -38.17536295476246266, 442.3073905683721136, -14.20200298773971426 ) ) ;
#20923 = ORIENTED_EDGE ( 'NONE', *, *, #10787, .F. ) ;
#20924 = CARTESIAN_POINT ( 'NONE',  ( -35.09675569278795848, 461.9948905683720000, -15.47720386886985544 ) ) ;
#20925 = CARTESIAN_POINT ( 'NONE',  ( -8.685887942688594876, 412.5573905601785896, -3.978247347592846594 ) ) ;
#20926 = CARTESIAN_POINT ( 'NONE',  ( -40.01497788969914637, 410.4323905765656377, -16.95518130045146421 ) ) ;
#20927 = FACE_OUTER_BOUND ( 'NONE', #1550, .T. ) ;
#20928 = PLANE ( 'NONE',  #10943 ) ;
#20929 = DIRECTION ( 'NONE',  ( -0.000000000000000000, -0.000000000000000000, 1.000000000000000000 ) ) ;
#20930 = CARTESIAN_POINT ( 'NONE',  ( -28.68588794268872633, 333.8848358243226357, 0.000000000000000000 ) ) ;
#20931 = CARTESIAN_POINT ( 'NONE',  ( -48.68588794268871567, 421.9948905765656377, 0.000000000000000000 ) ) ;
#20932 = CARTESIAN_POINT ( 'NONE',  ( -28.68588794268870146, 254.7448905601784475, -19.99999999999999289 ) ) ;
#20933 = EDGE_CURVE ( 'NONE', #17415, #10551, #15313, .T. ) ;
#20934 = ADVANCED_FACE ( 'NONE', ( #14242, #18763 ), #618, .T. ) ;
#20935 = CARTESIAN_POINT ( 'NONE',  ( -14.54375231895775222, 240.9948905601784759, 14.14213562373094568 ) ) ;
#20936 = LINE ( 'NONE', #11370, #1978 ) ;
#20937 = CARTESIAN_POINT ( 'NONE',  ( -42.88789093042844058, 424.4323905683720568, -9.489475012073736337 ) ) ;
#20938 = CARTESIAN_POINT ( 'NONE',  ( -17.35679799567829917, 383.8073905601784190, -16.95518130045146421 ) ) ;
#20939 = CARTESIAN_POINT ( 'NONE',  ( -32.01814843081343298, 253.1823905683720568, -16.75240474999999307 ) ) ;
#20940 = ORIENTED_EDGE ( 'NONE', *, *, #11483, .T. ) ;
#20941 = ORIENTED_EDGE ( 'NONE', *, *, #18151, .T. ) ;
#20942 = CARTESIAN_POINT ( 'NONE',  ( 20.42502041961806825, 281.1055109169419666, 40.00000000000000000 ) ) ;
#20943 = EDGE_LOOP ( 'NONE', ( #4144, #9253, #13292 ) ) ;
#20944 = CARTESIAN_POINT ( 'NONE',  ( -14.48388495494901029, 459.4323905683721136, 9.489475012073731008 ) ) ;
#20945 = CARTESIAN_POINT ( 'NONE',  ( -32.66413529028186247, 224.1823905765656377, 19.99999999999999289 ) ) ;
#20946 = ORIENTED_EDGE ( 'NONE', *, *, #15237, .T. ) ;
#20947 = CARTESIAN_POINT ( 'NONE',  ( 146.3141120573112630, 600.7448905601785327, 0.000000000000000000 ) ) ;
#20948 = CARTESIAN_POINT ( 'NONE',  ( -42.88789093042841927, 242.9323905683720284, -9.489475012073736337 ) ) ;
#20949 = ORIENTED_EDGE ( 'NONE', *, *, #18466, .T. ) ;
#20950 = CARTESIAN_POINT ( 'NONE',  ( 5.674999999999999822, 0.000000000000000000, 4.000000000000000000 ) ) ;
#20951 = LINE ( 'NONE', #21055, #13847 ) ;
#20952 = EDGE_CURVE ( 'NONE', #8903, #13483, #18865, .T. ) ;
#20953 = CIRCLE ( 'NONE', #21280, 4.400000000000000355 ) ;
#20954 = CARTESIAN_POINT ( 'NONE',  ( -8.685887942688736985, 467.3073905765656946, -3.978247347593165895 ) ) ;
#20955 = PLANE ( 'NONE',  #9955 ) ;
#20956 = CARTESIAN_POINT ( 'NONE',  ( -32.66413529028186247, 284.1823905765656377, 19.99999999999999289 ) ) ;
#20957 = CARTESIAN_POINT ( 'NONE',  ( -28.68588794268875120, 610.7448905601785327, 0.000000000000000000 ) ) ;
#20958 = PLANE ( 'NONE',  #11529 ) ;
#20959 = AXIS2_PLACEMENT_3D ( 'NONE', #4285, #19596, #16474 ) ;
#20960 = CARTESIAN_POINT ( 'NONE',  ( -9.656732250201606860, 223.9102039777117170, 6.363799471863218926 ) ) ;
#20961 = CARTESIAN_POINT ( 'NONE',  ( -42.88789093042841927, 224.8073905683720284, 9.489475012073736337 ) ) ;
#20962 = CARTESIAN_POINT ( 'NONE',  ( -19.19641293061497933, 311.9323905683720568, -14.20200298773971603 ) ) ;
#20963 = ADVANCED_FACE ( 'NONE', ( #10644 ), #17262, .T. ) ;
#20964 = DIRECTION ( 'NONE',  ( 1.000000000000000000, 1.191790137725560488E-16, 0.000000000000000000 ) ) ;
#20965 = CARTESIAN_POINT ( 'NONE',  ( -28.68588794268875120, 585.7448905601785327, 0.000000000000000000 ) ) ;
#20966 = CARTESIAN_POINT ( 'NONE',  ( -19.19641293061497933, 301.9323905683720000, -14.20200298773971603 ) ) ;
#20967 = AXIS2_PLACEMENT_3D ( 'NONE', #20965, #3223, #6448 ) ;
#20968 = CARTESIAN_POINT ( 'NONE',  ( -16.84014894278199037, 377.6198905683720568, 11.84573899990672530 ) ) ;
#20969 = CARTESIAN_POINT ( 'NONE',  ( -16.84014894278200813, 529.1198905683720568, 11.84573899990672530 ) ) ;
#20970 = CARTESIAN_POINT ( 'NONE',  ( -47.16347859291444422, 387.8698905601784759, 7.653668647301805628 ) ) ;
#20971 = CIRCLE ( 'NONE', #10590, 4.000000000000000000 ) ;
#20972 = CARTESIAN_POINT ( 'NONE',  ( -40.01497788969912506, 230.4323905765656093, -16.95518130045146421 ) ) ;
#20973 = ORIENTED_EDGE ( 'NONE', *, *, #10803, .T. ) ;
#20974 = ORIENTED_EDGE ( 'NONE', *, *, #8688, .T. ) ;
#20975 = CARTESIAN_POINT ( 'NONE',  ( -45.43829269268871940, 495.6823905683720568, 3.332260488124734632 ) ) ;
#20976 = DIRECTION ( 'NONE',  ( 0.000000000000000000, 0.000000000000000000, -1.000000000000000000 ) ) ;
#20977 = EDGE_LOOP ( 'NONE', ( #10800, #4632, #14013, #7355 ) ) ;
#20978 = CARTESIAN_POINT ( 'NONE',  ( -40.53162694259543031, 294.1198905683720568, -11.84573899990672707 ) ) ;
#20979 = CARTESIAN_POINT ( 'NONE',  ( -35.09675569278794427, 331.9948905683720000, -15.47720386886985544 ) ) ;
#20980 = CARTESIAN_POINT ( 'NONE',  ( -21.03221929538690205, 265.1198905765655809, 18.47759065022572500 ) ) ;
#20981 = DIRECTION ( 'NONE',  ( -1.000000000000000000, 0.000000000000000000, 0.000000000000000000 ) ) ;
#20982 = CARTESIAN_POINT ( 'NONE',  ( -42.88789093042841927, 234.8073905683720284, 9.489475012073734561 ) ) ;
#20983 = CARTESIAN_POINT ( 'NONE',  ( -32.01814843081345430, 403.1823905683720000, -16.75240474999999307 ) ) ;
#20984 = VECTOR ( 'NONE', #18049, 1000.000000000000114 ) ;
#20985 = FACE_OUTER_BOUND ( 'NONE', #2351, .T. ) ;
#20986 = CARTESIAN_POINT ( 'NONE',  ( 30.42502041961813575, 271.1055109169419097, 40.00000000000000000 ) ) ;
#20987 = PRODUCT_DEFINITION_SHAPE ( 'NONE', 'NONE',  #21400 ) ;
#20988 = EDGE_CURVE ( 'NONE', #15711, #18459, #13223, .T. ) ;
#20989 = CARTESIAN_POINT ( 'NONE',  ( -8.685887942688738761, 506.9948905765655240, -2.449293598294705724E-15 ) ) ;
#20990 = EDGE_CURVE ( 'NONE', #258, #13483, #16392, .T. ) ;
#20991 = CARTESIAN_POINT ( 'NONE',  ( -19.19641293061499354, 450.4323905683720000, -14.20200298773971603 ) ) ;
#20992 = CYLINDRICAL_SURFACE ( 'NONE', #9801, 19.99999999999999645 ) ;
#20993 = EDGE_LOOP ( 'NONE', ( #8528, #13125 ) ) ;
#20994 = CARTESIAN_POINT ( 'NONE',  ( -45.64106924314019409, 446.3073905601784759, -11.32908994701042715 ) ) ;
#20995 = ORIENTED_EDGE ( 'NONE', *, *, #2551, .T. ) ;
#20996 = ORIENTED_EDGE ( 'NONE', *, *, #9021, .F. ) ;
#20997 = VERTEX_POINT ( 'NONE', #1567 ) ;
#20998 = FACE_BOUND ( 'NONE', #20143, .T. ) ;
#20999 = CARTESIAN_POINT ( 'NONE',  ( -42.82802356641965247, 325.9948905601784759, -14.14213562373094746 ) ) ;
#21000 = DIRECTION ( 'NONE',  ( 0.000000000000000000, 0.000000000000000000, -1.000000000000000000 ) ) ;
#21001 = CARTESIAN_POINT ( 'NONE',  ( -40.53162694259543741, 354.1198905683720568, -11.84573899990672707 ) ) ;
#21002 = CARTESIAN_POINT ( 'NONE',  ( 0.5805565836007715586, -7.505553499465150935, -4.964436717930768604E-16 ) ) ;
#21003 = CARTESIAN_POINT ( 'NONE',  ( -28.68588794268872988, 494.4948905765656377, 19.99999999999999289 ) ) ;
#21004 = CARTESIAN_POINT ( 'NONE',  ( -38.17536295476246266, 392.3073905683720568, -14.20200298773971426 ) ) ;
#21005 = CARTESIAN_POINT ( 'NONE',  ( -13.20868407381884424, 229.7448905683720568, 6.410867750099229490 ) ) ;
#21006 = CARTESIAN_POINT ( 'NONE',  ( -19.19641293061498644, 407.3073905683719431, 14.20200298773971426 ) ) ;
#21007 = CARTESIAN_POINT ( 'NONE',  ( -48.68588794268870146, 322.3073905765656377, 3.978247347593168115 ) ) ;
#21008 = CARTESIAN_POINT ( 'NONE',  ( 91.21585410611801592, 31.85652257517428865, 40.00000000000000000 ) ) ;
#21009 = CARTESIAN_POINT ( 'NONE',  ( -32.01814843081344009, 296.0573905683720000, 16.75240474999999307 ) ) ;
#21010 =( NAMED_UNIT ( * ) PLANE_ANGLE_UNIT ( ) SI_UNIT ( $, .RADIAN. ) );
#21011 = CARTESIAN_POINT ( 'NONE',  ( -19.19641293061499354, 461.9323905683720568, -14.20200298773971603 ) ) ;
#21012 = LINE ( 'NONE', #10727, #17855 ) ;
#21013 = LINE ( 'NONE', #6182, #9351 ) ;
#21014 = CYLINDRICAL_SURFACE ( 'NONE', #3664, 19.99999999999999645 ) ;
#21015 =( BOUNDED_CURVE ( )  B_SPLINE_CURVE ( 2, ( #10289, #20472, #8886, #2090, #7046, #13666, #12026, #580, #20359, #15502, #5641, #1613, #11555, #10826, #20793, #6170, #1725 ),
 .UNSPECIFIED., .F., .T. ) 
 B_SPLINE_CURVE_WITH_KNOTS ( ( 3, 2, 2, 2, 2, 2, 2, 2, 3 ),
 ( 0.9531250000000001110, 0.9550781250000001110, 0.9570312500000001110, 0.9589843750000001110, 0.9609375000000001110, 0.9628906250000001110, 0.9648437500000001110, 0.9667968750000001110, 0.9687500000000001110 ),
 .UNSPECIFIED. ) 
 CURVE ( )  GEOMETRIC_REPRESENTATION_ITEM ( )  RATIONAL_B_SPLINE_CURVE ( ( 0.9999999999999988898, 0.9807852804032315408, 1.000000000000000000, 0.9807852804032304306, 1.000000000000000000, 0.9807852804032304306, 1.000000000000000000, 0.9807852804032304306, 1.000000000000000000, 0.9807852804032304306, 1.000000000000000000, 0.9807852804032304306, 1.000000000000000000, 0.9807852804032304306, 1.000000000000000000, 0.9807852804032293204, 1.000000000000001110 ) ) 
 REPRESENTATION_ITEM ( '' )  );
#21016 = CARTESIAN_POINT ( 'NONE',  ( -45.43829269268872650, 493.8698905683720568, 0.000000000000000000 ) ) ;
#21017 = CARTESIAN_POINT ( 'NONE',  ( -40.01497788969915348, 508.8073905601784190, 16.95518130045146776 ) ) ;
#21018 = CARTESIAN_POINT ( 'NONE',  ( -22.27502019258948351, 330.7448905683720568, -15.47720386886985544 ) ) ;
#21019 = VERTEX_POINT ( 'NONE', #11391 ) ;
#21020 = CARTESIAN_POINT ( 'NONE',  ( -11.73070664223726922, 523.1823905601784190, -11.32908994701042538 ) ) ;
#21021 = ORIENTED_EDGE ( 'NONE', *, *, #20274, .F. ) ;
#21022 = DIRECTION ( 'NONE',  ( -1.000000000000000000, -0.000000000000000000, 0.000000000000000000 ) ) ;
#21023 = AXIS2_PLACEMENT_3D ( 'NONE', #5253, #11852, #299 ) ;
#21024 = CARTESIAN_POINT ( 'NONE',  ( -45.43829269268871940, 425.0573905683720568, -3.332260488124726638 ) ) ;
#21025 = FACE_OUTER_BOUND ( 'NONE', #19931, .T. ) ;
#21026 = CARTESIAN_POINT ( 'NONE',  ( -42.88789093042844058, 442.9323905683721136, -9.489475012073736337 ) ) ;
#21027 = ORIENTED_EDGE ( 'NONE', *, *, #492, .F. ) ;
#21028 = CARTESIAN_POINT ( 'NONE',  ( -45.43829269268872650, 473.8698905683720568, 0.000000000000000000 ) ) ;
#21029 = PLANE ( 'NONE',  #2432 ) ;
#21030 = CARTESIAN_POINT ( 'NONE',  ( -32.66413529028187668, 374.1823905765655809, 19.99999999999999289 ) ) ;
#21031 = CARTESIAN_POINT ( 'NONE',  ( -45.64106924314017277, 281.0573905765656377, -11.32908994701042538 ) ) ;
#21032 = DIRECTION ( 'NONE',  ( 0.000000000000000000, 0.000000000000000000, 1.000000000000000000 ) ) ;
#21033 = CARTESIAN_POINT ( 'NONE',  ( -5.055092629213673101E-15, 5.469921996229795802, -3.525817189091416282 ) ) ;
#21034 = DIRECTION ( 'NONE',  ( 0.000000000000000000, 1.000000000000000000, 0.000000000000000000 ) ) ;
#21035 = VECTOR ( 'NONE', #18054, 1000.000000000000000 ) ;
#21036 = LINE ( 'NONE', #1251, #2323 ) ;
#21037 = DIRECTION ( 'NONE',  ( 1.000000000000000000, 0.000000000000000000, 0.000000000000000000 ) ) ;
#21038 = EDGE_CURVE ( 'NONE', #3421, #18163, #8369, .T. ) ;
#21039 = CARTESIAN_POINT ( 'NONE',  ( -44.87387987751963436, 223.9102039777115465, 7.648793815183834610 ) ) ;
#21040 = CIRCLE ( 'NONE', #4471, 20.00000000000000000 ) ;
#21041 = CARTESIAN_POINT ( 'NONE',  ( -14.48388495494900496, 429.4323905683720000, 9.489475012073732785 ) ) ;
#21042 = DIRECTION ( 'NONE',  ( -1.191790137725560488E-16, 1.000000000000000000, -0.000000000000000000 ) ) ;
#21043 = CARTESIAN_POINT ( 'NONE',  ( -14.48388495494898542, 241.3073905683720852, -9.489475012073736337 ) ) ;
#21044 = ORIENTED_EDGE ( 'NONE', *, *, #12063, .F. ) ;
#21045 = ORIENTED_EDGE ( 'NONE', *, *, #1652, .T. ) ;
#21046 = CARTESIAN_POINT ( 'NONE',  ( -24.70764059509555466, 424.8073905765656377, 19.99999999999998934 ) ) ;
#21047 = VERTEX_POINT ( 'NONE', #9346 ) ;
#21048 = CARTESIAN_POINT ( 'NONE',  ( -44.16309181155857999, 465.9948905683720000, 6.410867750099241924 ) ) ;
#21049 = CARTESIAN_POINT ( 'NONE',  ( -45.64106924314017277, 231.0573905765656093, -11.32908994701042715 ) ) ;
#21050 = ORIENTED_EDGE ( 'NONE', *, *, #8218, .F. ) ;
#21051 = CARTESIAN_POINT ( 'NONE',  ( -43.15102588740143119, 208.1950015687324651, 3.974285180378254179 ) ) ;
#21052 = CARTESIAN_POINT ( 'NONE',  ( -42.88789093042841927, 222.9323905683720284, -9.489475012073736337 ) ) ;
#21053 = EDGE_LOOP ( 'NONE', ( #20436, #506, #17843, #2374 ) ) ;
#21054 = CARTESIAN_POINT ( 'NONE',  ( -13.20868407381888154, 529.4948905683720568, -6.410867750099233042 ) ) ;
#21055 = CARTESIAN_POINT ( 'NONE',  ( 65.85920792673738333, 170.1716627696692683, 40.00000000000000000 ) ) ;
#21056 = VECTOR ( 'NONE', #16119, 1000.000000000000000 ) ;
#21057 = EDGE_CURVE ( 'NONE', #2116, #15898, #14768, .T. ) ;
#21058 = CARTESIAN_POINT ( 'NONE',  ( -32.66413529028188378, 434.1823905765656377, 19.99999999999999289 ) ) ;
#21059 = CARTESIAN_POINT ( 'NONE',  ( -17.35679799567828852, 350.6823905601785327, 16.95518130045146421 ) ) ;
#21060 = CARTESIAN_POINT ( 'NONE',  ( -40.01497788969912506, 283.5573905765656377, 16.95518130045146776 ) ) ;
#21061 = DIRECTION ( 'NONE',  ( 0.9283449136418786551, 0.000000000000000000, -0.3717199501173604204 ) ) ;
#21062 = DIRECTION ( 'NONE',  ( 1.000000000000000000, 1.250996701150283068E-16, -0.000000000000000000 ) ) ;
#21063 = CARTESIAN_POINT ( 'NONE',  ( -20.29731878304196968, 220.5357918889952771, -14.50086109035067317 ) ) ;
#21064 = CARTESIAN_POINT ( 'NONE',  ( -22.27502019258947996, 312.2448905683720000, -15.47720386886985544 ) ) ;
#21065 = DIRECTION ( 'NONE',  ( 0.000000000000000000, -1.000000000000000000, 0.000000000000000000 ) ) ;
#21066 = DIRECTION ( 'NONE',  ( -1.000000000000000000, -0.000000000000000000, -0.000000000000000000 ) ) ;
#21067 = CARTESIAN_POINT ( 'NONE',  ( -45.43829269268869808, 305.6823905683719431, 3.332260488124734632 ) ) ;
#21068 = EDGE_CURVE ( 'NONE', #9825, #13474, #2979, .T. ) ;
#21069 = CARTESIAN_POINT ( 'NONE',  ( -32.01814843081344719, 361.6823905683720568, -16.75240474999999307 ) ) ;
#21070 = CARTESIAN_POINT ( 'NONE',  ( -19.19641293061499709, 518.8073905683719431, 14.20200298773971426 ) ) ;
#21071 =( BOUNDED_CURVE ( )  B_SPLINE_CURVE ( 2, ( #1254, #7832, #16183, #7622, #1360, #7932, #6320, #6958, #8144, #8368, #6852, #11514, #21360, #18217, #6528, #284, #16720 ),
 .UNSPECIFIED., .F., .T. ) 
 B_SPLINE_CURVE_WITH_KNOTS ( ( 3, 2, 2, 2, 2, 2, 2, 2, 3 ),
 ( 0.8281250000000002220, 0.8300781250000002220, 0.8320312500000002220, 0.8339843750000002220, 0.8359375000000002220, 0.8378906250000002220, 0.8398437500000002220, 0.8417968750000002220, 0.8437500000000002220 ),
 .UNSPECIFIED. ) 
 CURVE ( )  GEOMETRIC_REPRESENTATION_ITEM ( )  RATIONAL_B_SPLINE_CURVE ( ( 0.9999999999999977796, 0.9807852804032326510, 1.000000000000000000, 0.9807852804032304306, 1.000000000000000000, 0.9807852804032304306, 1.000000000000000000, 0.9807852804032304306, 1.000000000000000000, 0.9807852804032304306, 1.000000000000000000, 0.9807852804032304306, 1.000000000000000000, 0.9807852804032304306, 1.000000000000000000, 0.9807852804032282101, 1.000000000000002220 ) ) 
 REPRESENTATION_ITEM ( '' )  );
#21072 = CARTESIAN_POINT ( 'NONE',  ( -47.16347859291444422, 367.8698905601784759, 7.653668647301805628 ) ) ;
#21073 = LINE ( 'NONE', #15897, #2889 ) ;
#21074 = EDGE_LOOP ( 'NONE', ( #11519, #2807, #15270, #14709, #1242, #13207 ) ) ;
#21075 = CARTESIAN_POINT ( 'NONE',  ( -35.09675569278796559, 487.2448905683720000, 15.47720386886985366 ) ) ;
#21076 = FACE_OUTER_BOUND ( 'NONE', #10766, .T. ) ;
#21077 = CARTESIAN_POINT ( 'NONE',  ( -11.93348319268871016, 278.8698905683720000, -2.051577885510841163E-15 ) ) ;
#21078 = VERTEX_POINT ( 'NONE', #9458 ) ;
#21079 = AXIS2_PLACEMENT_3D ( 'NONE', #4687, #16279, #11282 ) ;
#21080 = EDGE_CURVE ( 'NONE', #20702, #20033, #17680, .T. ) ;
#21081 = CARTESIAN_POINT ( 'NONE',  ( -42.88789093042842637, 284.4323905683720568, -9.489475012073734561 ) ) ;
#21082 = CARTESIAN_POINT ( 'NONE',  ( -22.27502019258947286, 316.9948905683720568, 15.47720386886985189 ) ) ;
#21083 = CARTESIAN_POINT ( 'NONE',  ( -11.73070664223723369, 256.0573905765656377, 11.32908994701042005 ) ) ;
#21084 = CARTESIAN_POINT ( 'NONE',  ( -8.685887942688735208, 472.2448905601784759, -2.449293598294705724E-15 ) ) ;
#21085 = CARTESIAN_POINT ( 'NONE',  ( -38.17536295476243424, 225.4323905683720000, 14.20200298773971781 ) ) ;
#21086 = CARTESIAN_POINT ( 'NONE',  ( -38.17536295476245556, 373.8073905683720000, -14.20200298773971426 ) ) ;
#21087 = CARTESIAN_POINT ( 'NONE',  ( 170.2047888904039610, 620.7448905601785327, -1.893624729818132124 ) ) ;
#21088 = AXIS2_PLACEMENT_3D ( 'NONE', #17148, #2539, #18970 ) ;
#21089 = DIRECTION ( 'NONE',  ( -0.000000000000000000, 0.000000000000000000, 1.000000000000000000 ) ) ;
#21090 = DIRECTION ( 'NONE',  ( -0.8090169943749473402, 0.000000000000000000, 0.5877852522924732481 ) ) ;
#21091 = CARTESIAN_POINT ( 'NONE',  ( -14.48388495494900852, 439.8073905683721136, -9.489475012073736337 ) ) ;
#21092 = LINE ( 'NONE', #11241, #2211 ) ;
#21093 = B_SPLINE_CURVE_WITH_KNOTS ( 'NONE', 3,
 ( #16071, #5780, #18978, #6096, #15964, #14453 ),
 .UNSPECIFIED., .F., .F.,
 ( 4, 2, 4 ),
 ( 2.380733003139562229E-07, 0.001898835937927372463, 0.003797433802554430696 ),
 .UNSPECIFIED. ) ;
#21094 = VERTEX_POINT ( 'NONE', #9767 ) ;
#21095 = CARTESIAN_POINT ( 'NONE',  ( -48.68588794268871567, 426.9323905601784759, -3.978247347593158345 ) ) ;
#21096 = ORIENTED_EDGE ( 'NONE', *, *, #19545, .F. ) ;
#21097 = VERTEX_POINT ( 'NONE', #12712 ) ;
#21098 = VERTEX_POINT ( 'NONE', #12609 ) ;
#21099 = CARTESIAN_POINT ( 'NONE',  ( -43.68588794268869435, 210.1437886375729249, -0.3278592396120701968 ) ) ;
#21100 = CARTESIAN_POINT ( 'NONE',  ( -40.01497788969913927, 335.6823905601784759, -16.95518130045146421 ) ) ;
#21101 = DIRECTION ( 'NONE',  ( -1.191790137725560488E-16, 1.000000000000000000, -0.000000000000000000 ) ) ;
#21102 = CARTESIAN_POINT ( 'NONE',  ( -25.35362745456398770, 342.5573905683721136, -16.75240474999999307 ) ) ;
#21103 = PRESENTATION_LAYER_ASSIGNMENT (  '', '', ( #9005 ) ) ;
#21104 = CIRCLE ( 'NONE', #17311, 6.500000000000000888 ) ;
#21105 = CARTESIAN_POINT ( 'NONE',  ( -40.01497788969915348, 503.5573905765656946, 16.95518130045146776 ) ) ;
#21106 = CARTESIAN_POINT ( 'NONE',  ( -32.01814843081345430, 391.6823905683720568, -16.75240474999999307 ) ) ;
#21107 = DIRECTION ( 'NONE',  ( 0.000000000000000000, 0.000000000000000000, -1.000000000000000000 ) ) ;
#21108 = EDGE_CURVE ( 'NONE', #10701, #16754, #4489, .T. ) ;
#21109 = CARTESIAN_POINT ( 'NONE',  ( -16.84014894278199392, 380.1198905683720568, -11.84573899990672707 ) ) ;
#21110 = CARTESIAN_POINT ( 'NONE',  ( -14.54375231895776466, 318.2448905765656377, -14.14213562373094746 ) ) ;
#21111 = CYLINDRICAL_SURFACE ( 'NONE', #8609, 15.00000000000000000 ) ;
#21112 = CARTESIAN_POINT ( 'NONE',  ( -45.43829269268870519, 293.5573905683720568, -3.332260488124726638 ) ) ;
#21113 = CARTESIAN_POINT ( 'NONE',  ( -38.17536295476246266, 433.8073905683720568, -14.20200298773971426 ) ) ;
#21114 = CARTESIAN_POINT ( 'NONE',  ( -8.685887942688712116, 282.2448905601784759, -2.449293598294705724E-15 ) ) ;
#21115 = CARTESIAN_POINT ( 'NONE',  ( -45.64106924314017988, 368.1823905601785327, 11.32908994701042538 ) ) ;
#21116 = CYLINDRICAL_SURFACE ( 'NONE', #5383, 19.99999999999999645 ) ;
#21117 = ADVANCED_FACE ( 'NONE', ( #1151 ), #6412, .T. ) ;
#21118 = CARTESIAN_POINT ( 'NONE',  ( -19.19641293061498644, 351.9323905683720568, -14.20200298773971603 ) ) ;
#21119 = CARTESIAN_POINT ( 'NONE',  ( -45.43829269268872650, 503.8698905683720568, 0.000000000000000000 ) ) ;
#21120 = EDGE_CURVE ( 'NONE', #827, #19850, #7722, .T. ) ;
#21121 = CARTESIAN_POINT ( 'NONE',  ( -32.66413529028189089, 505.0573905601784759, -19.99999999999999289 ) ) ;
#21122 = CARTESIAN_POINT ( 'NONE',  ( -14.48388495494899253, 317.9323905683720000, 9.489475012073732785 ) ) ;
#21123 = ADVANCED_FACE ( 'NONE', ( #14666 ), #2873, .F. ) ;
#21124 = ORIENTED_EDGE ( 'NONE', *, *, #9021, .T. ) ;
#21125 = CARTESIAN_POINT ( 'NONE',  ( -18.68588794268873698, 281.1055109169419666, -20.00000000000000355 ) ) ;
#21126 = ORIENTED_EDGE ( 'NONE', *, *, #14236, .F. ) ;
#21127 = FACE_OUTER_BOUND ( 'NONE', #3095, .T. ) ;
#21128 = CARTESIAN_POINT ( 'NONE',  ( -14.48388495494900674, 401.3073905683720000, -9.489475012073734561 ) ) ;
#21129 = CARTESIAN_POINT ( 'NONE',  ( -14.54375231895775222, 235.7448905765656093, 14.14213562373094568 ) ) ;
#21130 = SURFACE_STYLE_USAGE ( .BOTH. , #2863 ) ;
#21131 = CARTESIAN_POINT ( 'NONE',  ( -32.01814843081345430, 446.0573905683720568, 16.75240474999999307 ) ) ;
#21132 = ORIENTED_EDGE ( 'NONE', *, *, #21391, .F. ) ;
#21133 = CARTESIAN_POINT ( 'NONE',  ( -40.53162694259545162, 455.1198905683720568, 11.84573899990672885 ) ) ;
#21134 = DIRECTION ( 'NONE',  ( 0.9902947853249122190, 0.1389828700174457476, 0.000000000000000000 ) ) ;
#21135 = DIRECTION ( 'NONE',  ( -1.000000000000000000, 0.000000000000000000, 0.000000000000000000 ) ) ;
#21136 = EDGE_CURVE ( 'NONE', #4636, #18799, #13756, .T. ) ;
#21137 = CARTESIAN_POINT ( 'NONE',  ( -40.01497788969914637, 390.4323905765655809, -16.95518130045146421 ) ) ;
#21138 = CARTESIAN_POINT ( 'NONE',  ( -23.82219669152593156, 45.40396441825297558, 49.36459573994701344 ) ) ;
#21139 = VECTOR ( 'NONE', #13822, 1000.000000000000000 ) ;
#21140 = DIRECTION ( 'NONE',  ( -1.000000000000000000, -0.000000000000000000, -0.000000000000000000 ) ) ;
#21141 = CARTESIAN_POINT ( 'NONE',  ( -162.2727221670389781, 10.52886280891152104, 0.000000000000000000 ) ) ;
#21142 = VECTOR ( 'NONE', #17814, 1000.000000000000114 ) ;
#21143 = CARTESIAN_POINT ( 'NONE',  ( -14.48388495494901562, 491.3073905683720000, -9.489475012073736337 ) ) ;
#21144 = CARTESIAN_POINT ( 'NONE',  ( 60.69669829156632090, 56.85652257517428865, -94.99999999999994316 ) ) ;
#21145 = DIRECTION ( 'NONE',  ( 0.000000000000000000, 0.5000000000000007772, -0.8660254037844381525 ) ) ;
#21146 = CARTESIAN_POINT ( 'NONE',  ( -39.58131762249983154, 223.9102039777117170, 16.01692832265988642 ) ) ;
#21147 = CARTESIAN_POINT ( 'NONE',  ( -40.53162694259544452, 416.6198905683720000, 11.84573899990672885 ) ) ;
#21148 = CARTESIAN_POINT ( 'NONE',  ( -24.70764059509556176, 384.4323905601784190, -19.99999999999999289 ) ) ;
#21149 = CARTESIAN_POINT ( 'NONE',  ( -19.19641293061497223, 251.9323905683720284, -14.20200298773971603 ) ) ;
#21150 = ORIENTED_EDGE ( 'NONE', *, *, #13139, .F. ) ;
#21151 = EDGE_LOOP ( 'NONE', ( #9019, #12321, #20737, #10580 ) ) ;
#21152 = CYLINDRICAL_SURFACE ( 'NONE', #16204, 19.99999999999999645 ) ;
#21153 = EDGE_LOOP ( 'NONE', ( #18996, #20127, #15661, #4840, #10386, #13043, #1864 ) ) ;
#21154 = CARTESIAN_POINT ( 'NONE',  ( -22.27502019258949062, 468.4948905683720000, 15.47720386886985189 ) ) ;
#21155 = AXIS2_PLACEMENT_3D ( 'NONE', #13989, #12671, #1008 ) ;
#21156 = CARTESIAN_POINT ( 'NONE',  ( -21.03221929538690915, 228.8698905765655809, -18.47759065022572855 ) ) ;
#21157 = ORIENTED_EDGE ( 'NONE', *, *, #13520, .T. ) ;
#21158 = CARTESIAN_POINT ( 'NONE',  ( -13.20868407381887977, 529.7448905683720568, 6.410867750099229490 ) ) ;
#21159 = ORIENTED_EDGE ( 'NONE', *, *, #7140, .F. ) ;
#21160 = CARTESIAN_POINT ( 'NONE',  ( -25.35362745456401257, 531.0573905683719431, -16.75240474999999307 ) ) ;
#21161 = DIRECTION ( 'NONE',  ( -1.000000000000000000, 0.000000000000000000, 0.000000000000000000 ) ) ;
#21162 = CARTESIAN_POINT ( 'NONE',  ( -8.685887942688731655, 447.3073905765656377, -3.978247347593165895 ) ) ;
#21163 = PRODUCT_DEFINITION_SHAPE ( 'NONE', 'NONE',  #48 ) ;
#21164 = CARTESIAN_POINT ( 'NONE',  ( 4.700000000000000178, -5.629165124598843661, 3.250000000000012879 ) ) ;
#21165 = CARTESIAN_POINT ( 'NONE',  ( -11.93348319268872260, 339.1823905683720000, -3.332260488124732856 ) ) ;
#21166 = CARTESIAN_POINT ( 'NONE',  ( -32.66413529028188378, 454.1823905765656377, 19.99999999999999289 ) ) ;
#21167 = CARTESIAN_POINT ( 'NONE',  ( 5.299999999999999822, 0.000000000000000000, 0.000000000000000000 ) ) ;
#21168 = CARTESIAN_POINT ( 'NONE',  ( -8.685887942688802710, 291.9323905601784759, 3.978247347593374172 ) ) ;
#21169 = AXIS2_PLACEMENT_3D ( 'NONE', #13699, #5152, #1928 ) ;
#21170 = CARTESIAN_POINT ( 'NONE',  ( -11.06088464903279878, 213.9102039777116602, 5.773301668816275267 ) ) ;
#21171 = DIRECTION ( 'NONE',  ( 0.000000000000000000, -1.000000000000000000, 0.000000000000000000 ) ) ;
#21172 = CARTESIAN_POINT ( 'NONE',  ( -45.43829269268870519, 315.3698905683720568, 0.000000000000000000 ) ) ;
#21173 = CARTESIAN_POINT ( 'NONE',  ( -10.20829729246299600, 442.8698905601784759, -7.653668647301794969 ) ) ;
#21174 = DIRECTION ( 'NONE',  ( 0.000000000000000000, -1.000000000000000000, -0.000000000000000000 ) ) ;
#21175 = CARTESIAN_POINT ( 'NONE',  ( -35.09675569278793716, 313.4948905683720000, -15.47720386886985544 ) ) ;
#21176 = EDGE_CURVE ( 'NONE', #16109, #14968, #10788, .T. ) ;
#21177 = CARTESIAN_POINT ( 'NONE',  ( -45.43829269268873361, 515.6823905683720568, 3.332260488124734632 ) ) ;
#21178 = VECTOR ( 'NONE', #1271, 1000.000000000000000 ) ;
#21179 = CARTESIAN_POINT ( 'NONE',  ( -17.35679799567829917, 373.8073905601784759, -16.95518130045146421 ) ) ;
#21180 = DIRECTION ( 'NONE',  ( 1.000000000000000000, 0.000000000000000000, 0.000000000000000000 ) ) ;
#21181 = ORIENTED_EDGE ( 'NONE', *, *, #3336, .T. ) ;
#21182 = CARTESIAN_POINT ( 'NONE',  ( -45.43829269268872650, 485.3698905683720568, 0.000000000000000000 ) ) ;
#21183 = DIRECTION ( 'NONE',  ( -0.000000000000000000, 0.000000000000000000, 1.000000000000000000 ) ) ;
#21184 = CARTESIAN_POINT ( 'NONE',  ( -45.43829269268869808, 274.1823905683720000, 3.332260488124734632 ) ) ;
#21185 = VERTEX_POINT ( 'NONE', #9661 ) ;
#21186 = CARTESIAN_POINT ( 'NONE',  ( -28.68588794268870501, 282.8698905683720568, -16.75240474999999307 ) ) ;
#21187 = CARTESIAN_POINT ( 'NONE',  ( -38.17536295476245556, 332.3073905683720000, -14.20200298773971426 ) ) ;
#21188 = CARTESIAN_POINT ( 'NONE',  ( -11.93348319268870839, 260.6823905683720000, -3.332260488124732856 ) ) ;
#21189 = ADVANCED_FACE ( 'NONE', ( #16285 ), #1460, .T. ) ;
#21190 = AXIS2_PLACEMENT_3D ( 'NONE', #2270, #20220, #20434 ) ;
#21191 = CARTESIAN_POINT ( 'NONE',  ( -40.01497788969912506, 260.4323905765656377, -16.95518130045146421 ) ) ;
#21192 = PLANE ( 'NONE',  #20020 ) ;
#21193 = CARTESIAN_POINT ( 'NONE',  ( -35.09675569278793716, 225.7448905683720568, 15.47720386886985366 ) ) ;
#21194 = CARTESIAN_POINT ( 'NONE',  ( -28.68588794268874054, 573.2448905601785327, 0.000000000000000000 ) ) ;
#21195 = VECTOR ( 'NONE', #15065, 1000.000000000000000 ) ;
#21196 = CARTESIAN_POINT ( 'NONE',  ( -19.19641293061498288, 368.8073905683720000, 14.20200298773971426 ) ) ;
#21197 = DIRECTION ( 'NONE',  ( 0.000000000000000000, -0.000000000000000000, 1.000000000000000000 ) ) ;
#21198 = CARTESIAN_POINT ( 'NONE',  ( 21.30000000000000071, 0.000000000000000000, 0.000000000000000000 ) ) ;
#21199 = SHAPE_REPRESENTATION ( 'Heavy Arch Steel Frame Casting', ( #12794 ), #32 ) ;
#21200 = CARTESIAN_POINT ( 'NONE',  ( -21.03221929538691271, 268.8698905765656377, -18.47759065022572855 ) ) ;
#21201 = EDGE_CURVE ( 'NONE', #19679, #12430, #5230, .T. ) ;
#21202 = EDGE_CURVE ( 'NONE', #8258, #10793, #11829, .T. ) ;
#21203 = CARTESIAN_POINT ( 'NONE',  ( -16.84014894278199748, 430.1198905683720000, -11.84573899990672707 ) ) ;
#21204 = DIRECTION ( 'NONE',  ( -0.000000000000000000, -0.000000000000000000, 1.000000000000000000 ) ) ;
#21205 = EDGE_LOOP ( 'NONE', ( #20996, #3943, #11916, #16751, #13476, #10043 ) ) ;
#21206 = CARTESIAN_POINT ( 'NONE',  ( -36.33955658999051508, 435.3698905601784759, -18.47759065022572855 ) ) ;
#21207 = ORIENTED_EDGE ( 'NONE', *, *, #15987, .T. ) ;
#21208 = ORIENTED_EDGE ( 'NONE', *, *, #2280, .T. ) ;
#21209 = ORIENTED_EDGE ( 'NONE', *, *, #11957, .F. ) ;
#21210 = CARTESIAN_POINT ( 'NONE',  ( 10.41669750159067220, 217.7548513357008630, -45.00000000000000000 ) ) ;
#21211 = CARTESIAN_POINT ( 'NONE',  ( -32.66413529028186957, 305.0573905601784759, -19.99999999999999289 ) ) ;
#21212 = LINE ( 'NONE', #14839, #20429 ) ;
#21213 = VECTOR ( 'NONE', #5153, 1000.000000000000000 ) ;
#21214 = CARTESIAN_POINT ( 'NONE',  ( -25.35362745456397704, 338.1823905683720000, 16.75240474999998952 ) ) ;
#21215 = CARTESIAN_POINT ( 'NONE',  ( -48.68588794268872988, 512.3073905765655809, 3.978247347593168115 ) ) ;
#21216 = CARTESIAN_POINT ( 'NONE',  ( -40.53162694259543741, 375.1198905683720000, 11.84573899990672885 ) ) ;
#21217 = CARTESIAN_POINT ( 'NONE',  ( -28.68588794268869435, 227.8698905683720284, 16.75240474999999307 ) ) ;
#21218 = CARTESIAN_POINT ( 'NONE',  ( -16.84014894278199392, 390.1198905683720000, -11.84573899990672707 ) ) ;
#21219 = EDGE_CURVE ( 'NONE', #15264, #17415, #5015, .T. ) ;
#21220 = CARTESIAN_POINT ( 'NONE',  ( -21.03221929538690560, 325.1198905765655809, 18.47759065022572500 ) ) ;
#21221 = LINE ( 'NONE', #21008, #352 ) ;
#21222 = CARTESIAN_POINT ( 'NONE',  ( -40.53162694259543031, 285.1198905683720568, 11.84573899990672885 ) ) ;
#21223 = SHAPE_REPRESENTATION_RELATIONSHIP ( 'NONE' , 'NONE' ,  #8616, #16705 ) ;
#21224 = CARTESIAN_POINT ( 'NONE',  ( -16.84014894278200103, 441.6198905683720568, -11.84573899990672707 ) ) ;
#21225 = CARTESIAN_POINT ( 'NONE',  ( -32.66413529028186247, 285.0573905601784759, -19.99999999999999289 ) ) ;
#21226 = DIRECTION ( 'NONE',  ( 1.000000000000000000, 1.250996701150283068E-16, -0.000000000000000000 ) ) ;
#21227 = DIRECTION ( 'NONE',  ( -0.000000000000000000, 0.000000000000000000, 1.000000000000000000 ) ) ;
#21228 = CARTESIAN_POINT ( 'NONE',  ( -32.01814843081344719, 343.1823905683721136, -16.75240474999999307 ) ) ;
#21229 = CARTESIAN_POINT ( 'NONE',  ( -16.84014894278200103, 477.6198905683720000, 11.84573899990672530 ) ) ;
#21230 = CARTESIAN_POINT ( 'NONE',  ( -21.03221929538692336, 490.3698905601784759, 18.47759065022572500 ) ) ;
#21231 = CARTESIAN_POINT ( 'NONE',  ( -45.43829269268869808, 314.1823905683720000, 3.332260488124734632 ) ) ;
#21232 = ORIENTED_EDGE ( 'NONE', *, *, #8765, .F. ) ;
#21233 = CARTESIAN_POINT ( 'NONE',  ( -21.03221929538689849, 260.3698905601785327, 18.47759065022572500 ) ) ;
#21234 = ORIENTED_EDGE ( 'NONE', *, *, #14867, .T. ) ;
#21235 = DIRECTION ( 'NONE',  ( 0.000000000000000000, 0.000000000000000000, -1.000000000000000000 ) ) ;
#21236 = CARTESIAN_POINT ( 'NONE',  ( -22.27502019258947996, 398.4948905683720000, 15.47720386886985189 ) ) ;
#21237 = CARTESIAN_POINT ( 'NONE',  ( -47.16347859291443001, 232.6198905765656377, 7.653668647301805628 ) ) ;
#21238 = CARTESIAN_POINT ( 'NONE',  ( -28.68588794268875475, 600.7448905601785327, 0.000000000000000000 ) ) ;
#21239 = CARTESIAN_POINT ( 'NONE',  ( -32.01814843081345430, 441.6823905683721136, -16.75240474999999307 ) ) ;
#21240 = CARTESIAN_POINT ( 'NONE',  ( -45.43829269268871940, 444.1823905683719431, 3.332260488124734632 ) ) ;
#21241 = CARTESIAN_POINT ( 'NONE',  ( 6.416697501590684638, 217.7548513357008915, 69.47976867265059298 ) ) ;
#21242 = LINE ( 'NONE', #14449, #376 ) ;
#21243 = CARTESIAN_POINT ( 'NONE',  ( -8.685887942688722774, 377.3073905765656946, -3.978247347593165895 ) ) ;
#21244 = CARTESIAN_POINT ( 'NONE',  ( -19.19633154292390032, 45.73157677422673828, 48.68735826550700807 ) ) ;
#21245 = CARTESIAN_POINT ( 'NONE',  ( -17.35679799567829917, 388.5573905765656377, -16.95518130045146421 ) ) ;
#21246 = DIRECTION ( 'NONE',  ( 0.000000000000000000, 0.000000000000000000, -1.000000000000000000 ) ) ;
#21247 = CARTESIAN_POINT ( 'NONE',  ( -17.35679799567827786, 255.4323905765656377, 16.95518130045146421 ) ) ;
#21248 = CARTESIAN_POINT ( 'NONE',  ( -14.48388495494901740, 501.3073905683720568, -9.489475012073736337 ) ) ;
#21249 = FACE_OUTER_BOUND ( 'NONE', #17794, .T. ) ;
#21250 = DIRECTION ( 'NONE',  ( 1.191790137725560488E-16, -1.000000000000000000, -0.000000000000000000 ) ) ;
#21251 = CARTESIAN_POINT ( 'NONE',  ( -17.35679799567830628, 520.6823905601785327, 16.95518130045146421 ) ) ;
#21252 = CARTESIAN_POINT ( 'NONE',  ( -44.16309181155857999, 414.7448905683720568, -6.410867750099231266 ) ) ;
#21253 = CARTESIAN_POINT ( 'NONE',  ( -28.68588794268874054, 573.2448905601785327, 0.000000000000000000 ) ) ;
#21254 = CARTESIAN_POINT ( 'NONE',  ( -22.27502019258947286, 232.2448905683720000, -15.47720386886985544 ) ) ;
#21255 = EDGE_CURVE ( 'NONE', #15902, #13267, #11615, .T. ) ;
#21256 = ORIENTED_EDGE ( 'NONE', *, *, #4061, .T. ) ;
#21257 = ORIENTED_EDGE ( 'NONE', *, *, #18023, .T. ) ;
#21258 = CARTESIAN_POINT ( 'NONE',  ( -38.17536295476246977, 473.8073905683720000, -14.20200298773971426 ) ) ;
#21259 = CARTESIAN_POINT ( 'NONE',  ( -44.16309181155859420, 533.2448905683719431, -6.410867750099231266 ) ) ;
#21260 = ORIENTED_EDGE ( 'NONE', *, *, #17633, .F. ) ;
#21261 = DIRECTION ( 'NONE',  ( -1.000000000000000000, 0.000000000000000000, -0.000000000000000000 ) ) ;
#21262 = CARTESIAN_POINT ( 'NONE',  ( -40.53162694259542320, 225.1198905683720000, 11.84573899990672885 ) ) ;
#21263 = EDGE_LOOP ( 'NONE', ( #10705, #19770, #20887, #8236 ) ) ;
#21264 = CARTESIAN_POINT ( 'NONE',  ( -45.43829269268873361, 514.1823905683720568, 3.332260488124734632 ) ) ;
#21265 = CARTESIAN_POINT ( 'NONE',  ( 5.674999999999999822, -3.752776749732576356, -6.500000000000000000 ) ) ;
#21266 = CARTESIAN_POINT ( 'NONE',  ( -11.73070664223726034, 437.9323905765655809, -11.32908994701042715 ) ) ;
#21267 = CARTESIAN_POINT ( 'NONE',  ( -8.685887942688722774, 356.9948905765655809, -2.449293598294705724E-15 ) ) ;
#21268 = CARTESIAN_POINT ( 'NONE',  ( -14.54375231895775755, 248.2448905765656377, -14.14213562373094746 ) ) ;
#21269 =( NAMED_UNIT ( * ) PLANE_ANGLE_UNIT ( ) SI_UNIT ( $, .RADIAN. ) );
#21270 = DIRECTION ( 'NONE',  ( 0.000000000000000000, 1.000000000000000000, -0.000000000000000000 ) ) ;
#21271 = CARTESIAN_POINT ( 'NONE',  ( -45.64106924314017277, 288.1823905601785327, 11.32908994701042538 ) ) ;
#21272 = CARTESIAN_POINT ( 'NONE',  ( -19.19641293061496512, 227.3073905683720000, 14.20200298773971426 ) ) ;
#21273 = CARTESIAN_POINT ( 'NONE',  ( -42.88789093042842637, 326.3073905683721136, 9.489475012073736337 ) ) ;
#21274 = CARTESIAN_POINT ( 'NONE',  ( -32.66413529028187668, 445.0573905601784759, -19.99999999999999289 ) ) ;
#21275 = CARTESIAN_POINT ( 'NONE',  ( -14.54375231895775755, 263.4948905601784759, -14.14213562373094746 ) ) ;
#21276 = DIRECTION ( 'NONE',  ( 0.000000000000000000, 1.000000000000000000, 0.000000000000000000 ) ) ;
#21277 = CARTESIAN_POINT ( 'NONE',  ( -25.35362745456397349, 288.1823905683720000, 16.75240474999998952 ) ) ;
#21278 = CARTESIAN_POINT ( 'NONE',  ( -42.88789093042845479, 526.3073905683720568, 9.489475012073734561 ) ) ;
#21279 = CARTESIAN_POINT ( 'NONE',  ( -28.68588794268871212, 359.7448905601784759, 19.99999999999999289 ) ) ;
#21280 = AXIS2_PLACEMENT_3D ( 'NONE', #9432, #17763, #1331 ) ;
#21281 = CARTESIAN_POINT ( 'NONE',  ( 18.20947592957835326, 585.7448905601785327, -168.5995991907681457 ) ) ;
#21282 = ORIENTED_EDGE ( 'NONE', *, *, #5077, .F. ) ;
#21283 = CARTESIAN_POINT ( 'NONE',  ( -35.09675569278796559, 477.2448905683720568, 15.47720386886985366 ) ) ;
#21284 = DIRECTION ( 'NONE',  ( 1.000000000000000000, 0.000000000000000000, 0.000000000000000000 ) ) ;
#21285 = CARTESIAN_POINT ( 'NONE',  ( -14.48388495494899075, 279.8073905683720000, -9.489475012073736337 ) ) ;
#21286 = ORIENTED_EDGE ( 'NONE', *, *, #20876, .F. ) ;
#21287 = CARTESIAN_POINT ( 'NONE',  ( -14.48388495494899075, 281.3073905683720000, -9.489475012073734561 ) ) ;
#21288 = VECTOR ( 'NONE', #5158, 1000.000000000000000 ) ;
#21289 = CARTESIAN_POINT ( 'NONE',  ( -28.68588794268870856, 311.3698905683720568, -16.75240474999999307 ) ) ;
#21290 = CARTESIAN_POINT ( 'NONE',  ( -36.33955658999050087, 253.8698905765656093, 18.47759065022572500 ) ) ;
#21291 = DIRECTION ( 'NONE',  ( 1.000000000000000000, 0.000000000000000000, 0.000000000000000000 ) ) ;
#21292 = CARTESIAN_POINT ( 'NONE',  ( -13.20868407381884602, 229.4948905683720284, -6.410867750099233042 ) ) ;
#21293 = EDGE_CURVE ( 'NONE', #11997, #2086, #16817, .T. ) ;
#21294 = CARTESIAN_POINT ( 'NONE',  ( -38.17536295476245556, 383.8073905683720568, -14.20200298773971426 ) ) ;
#21295 = VECTOR ( 'NONE', #10127, 1000.000000000000000 ) ;
#21296 = CARTESIAN_POINT ( 'NONE',  ( -42.82802356641963826, 204.8148611821455916, 5.000000000000001776 ) ) ;
#21297 = FACE_OUTER_BOUND ( 'NONE', #2067, .T. ) ;
#21298 = ADVANCED_FACE ( 'NONE', ( #1793 ), #15197, .T. ) ;
#21299 = DIRECTION ( 'NONE',  ( -1.191790137725560488E-16, 1.000000000000000000, -0.000000000000000000 ) ) ;
#21300 = AXIS2_PLACEMENT_3D ( 'NONE', #14930, #18869, #7613 ) ;
#21301 = CARTESIAN_POINT ( 'NONE',  ( -25.35362745456399836, 421.0573905683720000, -16.75240474999999307 ) ) ;
#21302 = UNCERTAINTY_MEASURE_WITH_UNIT (LENGTH_MEASURE( 1.000000000000000082E-05 ), #15423, 'distance_accuracy_value', 'NONE');
#21303 = CARTESIAN_POINT ( 'NONE',  ( 116.0391604516428430, 192.9550247130592027, 40.00000000000000000 ) ) ;
#21304 = ORIENTED_EDGE ( 'NONE', *, *, #15522, .F. ) ;
#21305 = CARTESIAN_POINT ( 'NONE',  ( -17.35679799567830628, 433.8073905601784759, -16.95518130045146421 ) ) ;
#21306 = ORIENTED_EDGE ( 'NONE', *, *, #3594, .F. ) ;
#21307 = ORIENTED_EDGE ( 'NONE', *, *, #14792, .F. ) ;
#21308 = VERTEX_POINT ( 'NONE', #16496 ) ;
#21309 = CARTESIAN_POINT ( 'NONE',  ( -14.54375231895776643, 355.7448905765655809, 14.14213562373094568 ) ) ;
#21310 = CARTESIAN_POINT ( 'NONE',  ( -47.16347859291443712, 297.8698905601784759, 7.653668647301805628 ) ) ;
#21311 = DIRECTION ( 'NONE',  ( 0.000000000000000000, 1.000000000000000000, -0.000000000000000000 ) ) ;
#21312 = CARTESIAN_POINT ( 'NONE',  ( -11.93348319268871904, 340.3698905683720000, -2.051577885510841163E-15 ) ) ;
#21313 = AXIS2_PLACEMENT_3D ( 'NONE', #2443, #15647, #833 ) ;
#21314 = CARTESIAN_POINT ( 'NONE',  ( -47.16347859291445843, 481.3698905765655809, -7.653668647301793193 ) ) ;
#21315 = CARTESIAN_POINT ( 'NONE',  ( -44.16309181155856578, 374.4948905683720000, 6.410867750099241924 ) ) ;
#21316 = CARTESIAN_POINT ( 'NONE',  ( -19.19641293061496512, 228.8073905683720284, 14.20200298773971426 ) ) ;
#21317 = CARTESIAN_POINT ( 'NONE',  ( -32.01814843081344719, 391.6823905683720568, -16.75240474999999307 ) ) ;
#21318 = EDGE_CURVE ( 'NONE', #18850, #17724, #2102, .T. ) ;
#21319 = CIRCLE ( 'NONE', #14438, 38.00000000000000000 ) ;
#21320 = CARTESIAN_POINT ( 'NONE',  ( -21.03221929538690560, 315.1198905765656377, 18.47759065022572500 ) ) ;
#21321 = CARTESIAN_POINT ( 'NONE',  ( -24.70764059509556532, 424.4323905601785327, -19.99999999999999289 ) ) ;
#21322 = CARTESIAN_POINT ( 'NONE',  ( -13.20868407381884779, 278.2448905683720568, 6.410867750099229490 ) ) ;
#21323 = DIRECTION ( 'NONE',  ( -1.000000000000000000, 0.000000000000000000, 0.000000000000000000 ) ) ;
#21324 = ADVANCED_BREP_SHAPE_REPRESENTATION ( '', ( #4508, #12794 ), #14893 ) ;
#21325 =( BOUNDED_CURVE ( )  B_SPLINE_CURVE ( 3, ( #5053, #12164, #18247, #17041 ),
 .UNSPECIFIED., .F., .T. ) 
 B_SPLINE_CURVE_WITH_KNOTS ( ( 4, 4 ),
 ( 3.141592653589793116, 4.712388980384687898 ),
 .UNSPECIFIED. ) 
 CURVE ( )  GEOMETRIC_REPRESENTATION_ITEM ( )  RATIONAL_B_SPLINE_CURVE ( ( 1.000000000000000000, 0.8047378541243654926, 0.8047378541243654926, 1.000000000000000000 ) ) 
 REPRESENTATION_ITEM ( '' )  );
#21326 = CARTESIAN_POINT ( 'NONE',  ( -19.19641293061498999, 431.9323905683719431, -14.20200298773971603 ) ) ;
#21327 = CARTESIAN_POINT ( 'NONE',  ( -28.68588794268874409, 608.2448905601786464, 0.000000000000000000 ) ) ;
#21328 = CARTESIAN_POINT ( 'NONE',  ( -11.73070664223726745, 513.1823905601785327, -11.32908994701042538 ) ) ;
#21329 = DIRECTION ( 'NONE',  ( -0.000000000000000000, -0.000000000000000000, 1.000000000000000000 ) ) ;
#21330 = CARTESIAN_POINT ( 'NONE',  ( -48.68588794268877251, 447.5573905601785327, 3.978247347593061978 ) ) ;
#21331 = AXIS2_PLACEMENT_3D ( 'NONE', #10035, #5065, #8305 ) ;
#21332 = CARTESIAN_POINT ( 'NONE',  ( -44.16309181155857289, 344.7448905683720568, -6.410867750099231266 ) ) ;
#21333 = CARTESIAN_POINT ( 'NONE',  ( -35.09675569278796559, 485.7448905683720568, 15.47720386886985366 ) ) ;
#21334 = ORIENTED_EDGE ( 'NONE', *, *, #10537, .F. ) ;
#21335 = CARTESIAN_POINT ( 'NONE',  ( -40.01497788969914637, 488.8073905601784759, 16.95518130045146776 ) ) ;
#21336 = CARTESIAN_POINT ( 'NONE',  ( -44.16309181155855867, 304.4948905683720568, 6.410867750099241924 ) ) ;
#21337 = EDGE_CURVE ( 'NONE', #12056, #10333, #11931, .T. ) ;
#21338 = AXIS2_PLACEMENT_3D ( 'NONE', #13732, #17083, #2158 ) ;
#21339 = ORIENTED_EDGE ( 'NONE', *, *, #19267, .T. ) ;
#21340 = CARTESIAN_POINT ( 'NONE',  ( 0.5805565836007597902, 3.752776749732560368, -6.499999999999999112 ) ) ;
#21341 = PRODUCT_DEFINITION_SHAPE ( 'NONE', 'NONE',  #21406 ) ;
#21342 = ORIENTED_EDGE ( 'NONE', *, *, #20031, .F. ) ;
#21343 = CARTESIAN_POINT ( 'NONE',  ( -40.53162694259544452, 404.1198905683720000, -11.84573899990672707 ) ) ;
#21344 = CARTESIAN_POINT ( 'NONE',  ( -48.68588794268885778, 477.5573905601784759, 3.978247347592849259 ) ) ;
#21345 = DIRECTION ( 'NONE',  ( -1.000000000000000000, 0.000000000000000000, 0.000000000000000000 ) ) ;
#21346 = CARTESIAN_POINT ( 'NONE',  ( -35.09675569278795848, 445.7448905683720000, 15.47720386886985366 ) ) ;
#21347 = CARTESIAN_POINT ( 'NONE',  ( -16.84014894278200103, 440.1198905683720568, -11.84573899990672707 ) ) ;
#21348 = CARTESIAN_POINT ( 'NONE',  ( -32.66413529028187668, 415.0573905601784759, -19.99999999999999289 ) ) ;
#21349 = EDGE_CURVE ( 'NONE', #5796, #13961, #13573, .T. ) ;
#21350 = CARTESIAN_POINT ( 'NONE',  ( -11.73070664223725146, 386.0573905765656946, 11.32908994701042005 ) ) ;
#21351 = CARTESIAN_POINT ( 'NONE',  ( -11.50723138933277490, 52.75769294733686365, 46.53163365174636112 ) ) ;
#21352 = CARTESIAN_POINT ( 'NONE',  ( -28.68588794268874054, 573.2448905601785327, 0.000000000000000000 ) ) ;
#21353 = DIRECTION ( 'NONE',  ( 0.000000000000000000, 0.000000000000000000, 1.000000000000000000 ) ) ;
#21354 = CARTESIAN_POINT ( 'NONE',  ( -10.20829729246300133, 487.6198905765656377, -7.653668647301794969 ) ) ;
#21355 = CARTESIAN_POINT ( 'NONE',  ( -32.01814843081346140, 487.5573905683720568, 16.75240474999999307 ) ) ;
#21356 = CARTESIAN_POINT ( 'NONE',  ( -54.57497958038185715, 303.6587712403113528, 25.00000000000000000 ) ) ;
#21357 = PRESENTATION_STYLE_ASSIGNMENT (( #3614 ) ) ;
#21358 = LINE ( 'NONE', #3509, #408 ) ;
#21359 = CARTESIAN_POINT ( 'NONE',  ( -25.35362745456399480, 402.5573905683720000, -16.75240474999999307 ) ) ;
#21360 = CARTESIAN_POINT ( 'NONE',  ( -42.82802356641964536, 263.2448905765656377, 14.14213562373094923 ) ) ;
#21361 = CARTESIAN_POINT ( 'NONE',  ( -11.93348319268870661, 230.0573905683720284, 3.332260488124728415 ) ) ;
#21362 = AXIS2_PLACEMENT_3D ( 'NONE', #11211, #14047, #14265 ) ;
#21363 = ORIENTED_EDGE ( 'NONE', *, *, #10887, .T. ) ;
#21364 = PLANE ( 'NONE',  #7879 ) ;
#21365 = VERTEX_POINT ( 'NONE', #6952 ) ;
#21366 = CARTESIAN_POINT ( 'NONE',  ( -45.43829269268871940, 445.0573905683720000, -3.332260488124726638 ) ) ;
#21367 = CARTESIAN_POINT ( 'NONE',  ( -17.35679799567827786, 235.4323905765656093, 16.95518130045146421 ) ) ;
#21368 = CIRCLE ( 'NONE', #2696, 20.00000000000000000 ) ;
#21369 = VERTEX_POINT ( 'NONE', #20163 ) ;
#21370 = PLANE ( 'NONE',  #40 ) ;
#21371 = CARTESIAN_POINT ( 'NONE',  ( -14.48388495494898187, 227.9323905683720000, 9.489475012073732785 ) ) ;
#21372 = ORIENTED_EDGE ( 'NONE', *, *, #3622, .F. ) ;
#21373 = CARTESIAN_POINT ( 'NONE',  ( -38.17536295476246977, 502.3073905683720568, -14.20200298773971426 ) ) ;
#21374 = CARTESIAN_POINT ( 'NONE',  ( 20.42502041961813930, 230.5765313837437418, -40.00000000000000000 ) ) ;
#21375 = CARTESIAN_POINT ( 'NONE',  ( -8.685887942688729879, 436.9948905765656377, -2.449293598294705724E-15 ) ) ;
#21376 = CARTESIAN_POINT ( 'NONE',  ( -36.33955658999050797, 360.1198905765656377, -18.47759065022572855 ) ) ;
#21377 = CARTESIAN_POINT ( 'NONE',  ( -45.64106924314016567, 251.0573905765656093, -11.32908994701042538 ) ) ;
#21378 = CYLINDRICAL_SURFACE ( 'NONE', #12559, 19.99999999999999645 ) ;
#21379 = CARTESIAN_POINT ( 'NONE',  ( 0.5805565836007647862, -3.752776749732576356, -6.500000000000000000 ) ) ;
#21380 = EDGE_CURVE ( 'NONE', #15268, #14922, #15150, .T. ) ;
#21381 = CARTESIAN_POINT ( 'NONE',  ( -10.20829729246297646, 291.6198905601784759, 7.653668647301790529 ) ) ;
#21382 = VECTOR ( 'NONE', #4376, 1000.000000000000000 ) ;
#21383 = EDGE_CURVE ( 'NONE', #12217, #20490, #19726, .T. ) ;
#21384 = CARTESIAN_POINT ( 'NONE',  ( -14.80883852731595596, 223.9102039777117170, 14.49255704181644866 ) ) ;
#21385 = LINE ( 'NONE', #18025, #5566 ) ;
#21386 = CARTESIAN_POINT ( 'NONE',  ( -45.43829269268869808, 315.6823905683720000, 3.332260488124734632 ) ) ;
#21387 = PLANE ( 'NONE',  #11274 ) ;
#21388 = CARTESIAN_POINT ( 'NONE',  ( -42.82802356641965247, 275.9948905601785327, -14.14213562373094746 ) ) ;
#21389 = CARTESIAN_POINT ( 'NONE',  ( -33.84809828339279392, 56.37865086801084402, -49.33155846391707655 ) ) ;
#21390 = CARTESIAN_POINT ( 'NONE',  ( -42.88789093042842637, 284.4323905683720000, -9.489475012073736337 ) ) ;
#21391 = EDGE_CURVE ( 'NONE', #20120, #18164, #12107, .T. ) ;
#21392 = CARTESIAN_POINT ( 'NONE',  ( -48.68588794268873698, 573.2448905601785327, 0.000000000000000000 ) ) ;
#21393 = NEXT_ASSEMBLY_USAGE_OCCURRENCE ( 'NAUO1', ' ', ' ', #19867, #15858, $ ) ;
#21394 = NEXT_ASSEMBLY_USAGE_OCCURRENCE ( 'NAUO2', ' ', ' ', #19867, #4341, $ ) ;
#21395 = NEXT_ASSEMBLY_USAGE_OCCURRENCE ( 'NAUO3', ' ', ' ', #19867, #11071, $ ) ;
#21396 = NEXT_ASSEMBLY_USAGE_OCCURRENCE ( 'NAUO4', ' ', ' ', #19867, #18472, $ ) ;
#21397 = NEXT_ASSEMBLY_USAGE_OCCURRENCE ( 'NAUO5', ' ', ' ', #19867, #7228, $ ) ;
#21398 = NEXT_ASSEMBLY_USAGE_OCCURRENCE ( 'NAUO6', ' ', ' ', #19867, #5449, $ ) ;
#21399 = NEXT_ASSEMBLY_USAGE_OCCURRENCE ( 'NAUO7', ' ', ' ', #19867, #324, $ ) ;
#21400 = NEXT_ASSEMBLY_USAGE_OCCURRENCE ( 'NAUO8', ' ', ' ', #19867, #5449, $ ) ;
#21401 = NEXT_ASSEMBLY_USAGE_OCCURRENCE ( 'NAUO9', ' ', ' ', #19867, #48, $ ) ;
#21402 = NEXT_ASSEMBLY_USAGE_OCCURRENCE ( 'NAUO10', ' ', ' ', #19867, #48, $ ) ;
#21403 = NEXT_ASSEMBLY_USAGE_OCCURRENCE ( 'NAUO11', ' ', ' ', #19867, #48, $ ) ;
#21404 = NEXT_ASSEMBLY_USAGE_OCCURRENCE ( 'NAUO12', ' ', ' ', #19867, #8621, $ ) ;
#21405 = NEXT_ASSEMBLY_USAGE_OCCURRENCE ( 'NAUO13', ' ', ' ', #19867, #8621, $ ) ;
#21406 = NEXT_ASSEMBLY_USAGE_OCCURRENCE ( 'NAUO14', ' ', ' ', #19867, #8621, $ ) ;
#21407 = NEXT_ASSEMBLY_USAGE_OCCURRENCE ( 'NAUO15', ' ', ' ', #19867, #8621, $ ) ;
#21408=COLOUR_RGB('Dark Blue',0.08,0.2,0.34);
#21409=FILL_AREA_STYLE_COLOUR('',#21408);
#21410=FILL_AREA_STYLE('',(#21409));
#21411=SURFACE_STYLE_FILL_AREA(#21410);
#21412=SURFACE_SIDE_STYLE('',(#21411));
#21413=SURFACE_STYLE_USAGE(.BOTH.,#21412);
#21414=PRESENTATION_STYLE_ASSIGNMENT((#21413));
#21415=COLOUR_RGB('Light Blue',0.38,0.62,0.78);
#21416=FILL_AREA_STYLE_COLOUR('',#21415);
#21417=FILL_AREA_STYLE('',(#21416));
#21418=SURFACE_STYLE_FILL_AREA(#21417);
#21419=SURFACE_SIDE_STYLE('',(#21418));
#21420=SURFACE_STYLE_USAGE(.BOTH.,#21419);
#21421=PRESENTATION_STYLE_ASSIGNMENT((#21420));
#21422=COLOUR_RGB('Sky Blue',0.24,0.69,0.87);
#21423=FILL_AREA_STYLE_COLOUR('',#21422);
#21424=FILL_AREA_STYLE('',(#21423));
#21425=SURFACE_STYLE_FILL_AREA(#21424);
#21426=SURFACE_SIDE_STYLE('',(#21425));
#21427=SURFACE_STYLE_USAGE(.BOTH.,#21426);
#21428=PRESENTATION_STYLE_ASSIGNMENT((#21427));
#21429=COLOUR_RGB('Grey',0.48,0.52,0.57);
#21430=FILL_AREA_STYLE_COLOUR('',#21429);
#21431=FILL_AREA_STYLE('',(#21430));
#21432=SURFACE_STYLE_FILL_AREA(#21431);
#21433=SURFACE_SIDE_STYLE('',(#21432));
#21434=SURFACE_STYLE_USAGE(.BOTH.,#21433);
#21435=PRESENTATION_STYLE_ASSIGNMENT((#21434));
#21436=COLOUR_RGB('Black',0.12,0.14,0.17);
#21437=FILL_AREA_STYLE_COLOUR('',#21436);
#21438=FILL_AREA_STYLE('',(#21437));
#21439=SURFACE_STYLE_FILL_AREA(#21438);
#21440=SURFACE_SIDE_STYLE('',(#21439));
#21441=SURFACE_STYLE_USAGE(.BOTH.,#21440);
#21442=PRESENTATION_STYLE_ASSIGNMENT((#21441));
#21443=COLOUR_RGB('Off White',0.89,0.88,0.83);
#21444=FILL_AREA_STYLE_COLOUR('',#21443);
#21445=FILL_AREA_STYLE('',(#21444));
#21446=SURFACE_STYLE_FILL_AREA(#21445);
#21447=SURFACE_SIDE_STYLE('',(#21446));
#21448=SURFACE_STYLE_USAGE(.BOTH.,#21447);
#21449=PRESENTATION_STYLE_ASSIGNMENT((#21448));
ENDSEC;
END-ISO-10303-21;
